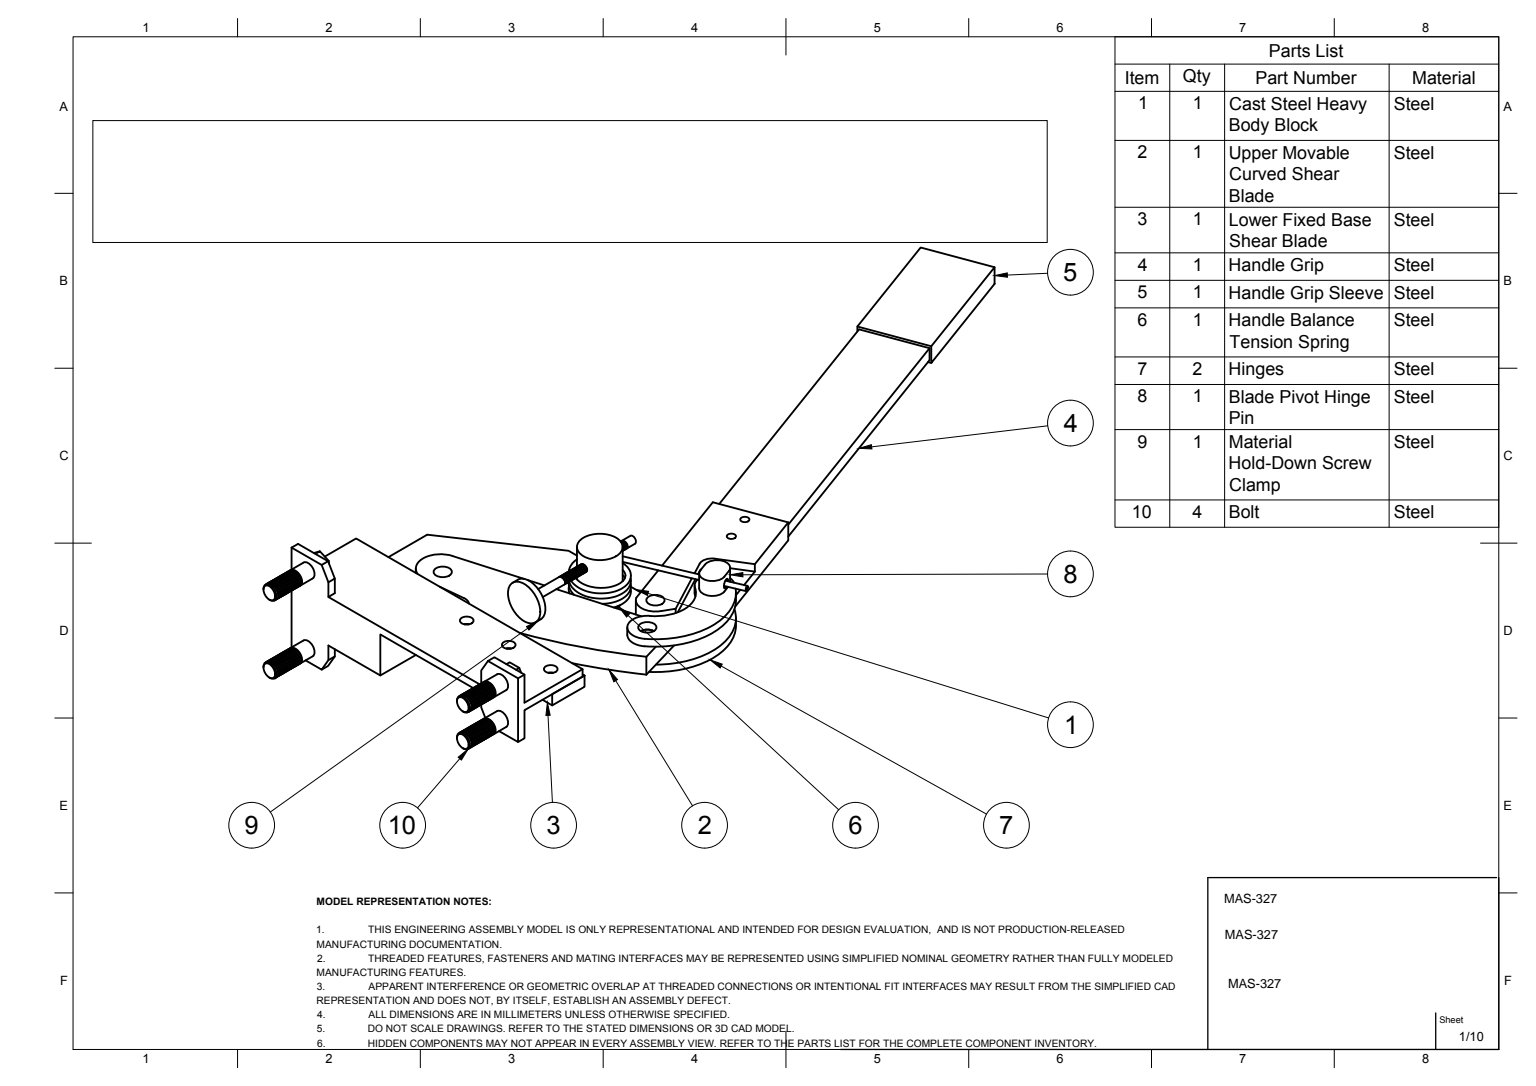
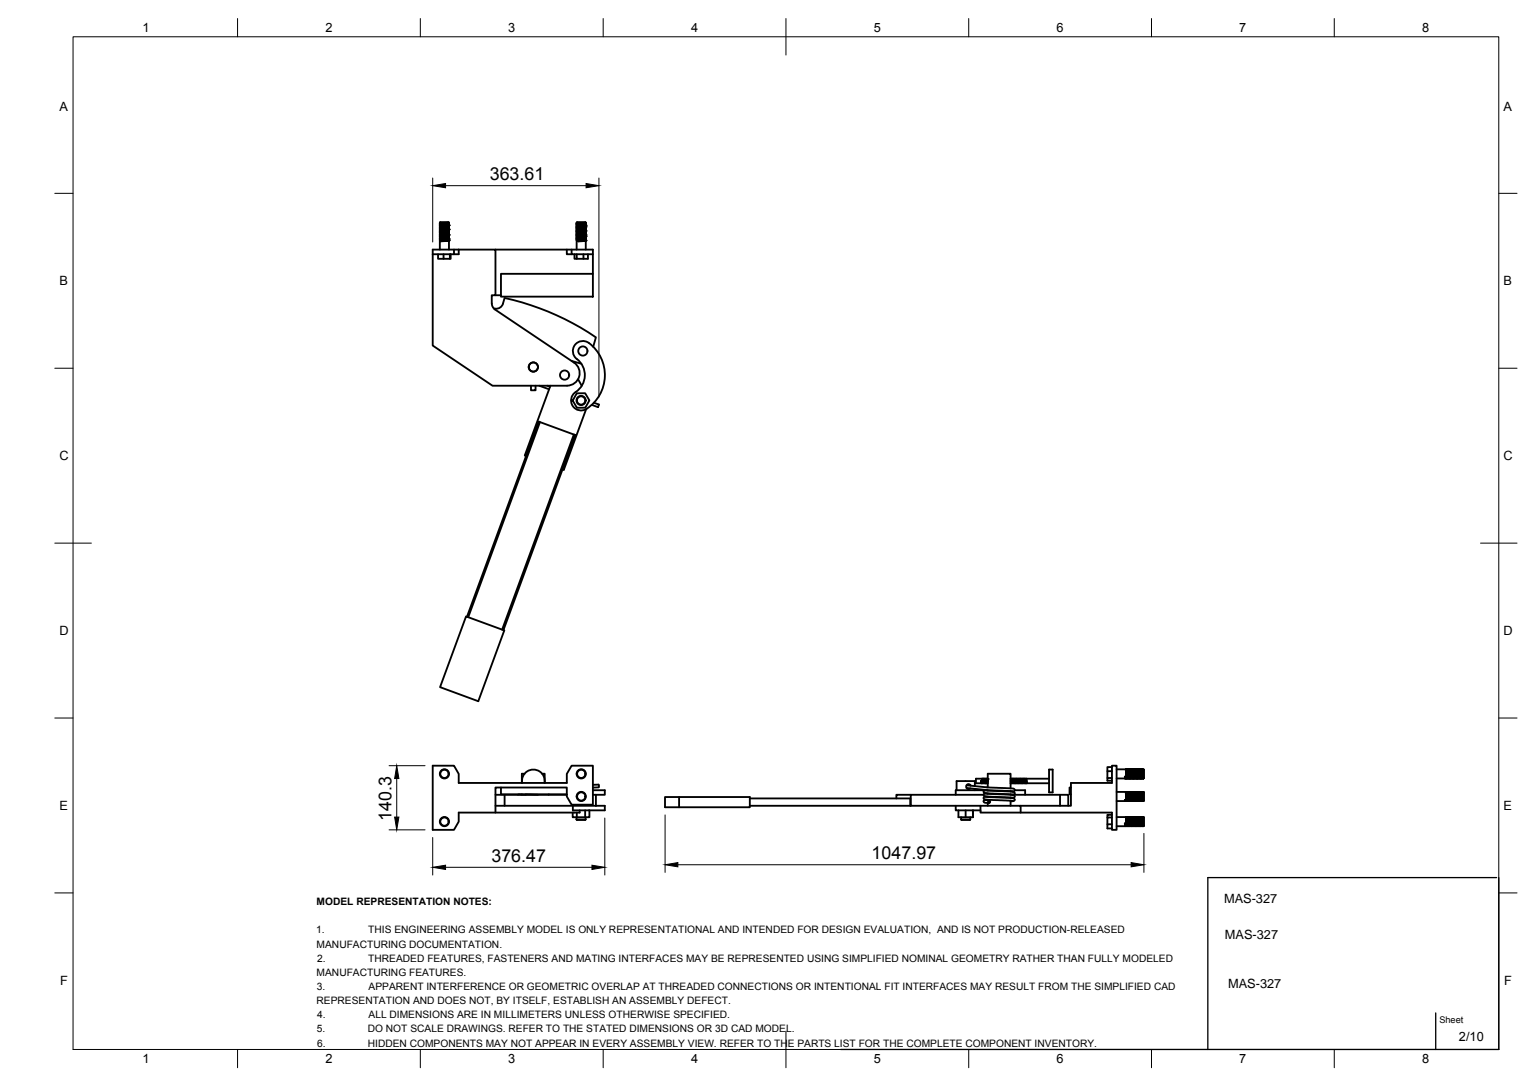
ISO-10303-21;
HEADER;
FILE_DESCRIPTION (('STEP AP214'),
    '1' );
FILE_NAME ('MAS-327',
    '2026-10-06T22:16:42',
    ( '' ),
    ( '' ),
    'SwSTEP 2.0',
    'SolidWorks 2025',
    '' );
FILE_SCHEMA (( 'AUTOMOTIVE_DESIGN' ));
ENDSEC;

DATA;
#1 = CARTESIAN_POINT ( 'NONE',  ( -157.2955611005345986, -176.6084106276440195, 41.63779006702063867 ) ) ;
#2 = ORIENTED_EDGE ( 'NONE', *, *, #5010, .T. ) ;
#3 = CARTESIAN_POINT ( 'NONE',  ( 41.64333658814960870, 63.71518717409399812, 38.42115945441014446 ) ) ;
#4 = CARTESIAN_POINT ( 'NONE',  ( -160.8964159109769696, -164.1584106276440593, 49.65701158161630957 ) ) ;
#5 = CARTESIAN_POINT ( 'NONE',  ( 71.26135857449716582, 118.5824631887579272, 4.723566274445706092 ) ) ;
#6 = FILL_AREA_STYLE_COLOUR ( '', #17600 ) ;
#7 = CARTESIAN_POINT ( 'NONE',  ( 40.27526882409969033, 126.5651871740940209, 37.97664729208901946 ) ) ;
#8 = VERTEX_POINT ( 'NONE', #17420 ) ;
#9 = ORIENTED_EDGE ( 'NONE', *, *, #6823, .T. ) ;
#10 = AXIS2_PLACEMENT_3D ( 'NONE', #19848, #7848, #14551 ) ;
#11 = CARTESIAN_POINT ( 'NONE',  ( -141.4692556286852891, -192.9891397928654726, 49.65701158161630957 ) ) ;
#12 = EDGE_LOOP ( 'NONE', ( #7089, #16124, #17025, #12845, #13237 ) ) ;
#13 = CARTESIAN_POINT ( 'NONE',  ( 41.46631938032478359, 107.1844580088725820, 29.45539723777780239 ) ) ;
#14 = CARTESIAN_POINT ( 'NONE',  ( 38.58424406990786082, 153.3797705074273097, 34.21067981925357060 ) ) ;
#15 = CARTESIAN_POINT ( 'NONE',  ( 44.37947211624943833, 71.47977050742731819, 30.00020018409699318 ) ) ;
#17 = CARTESIAN_POINT ( 'NONE',  ( 22.10153057061799231, 100.9866247252079745, 1.346821830042071566 ) ) ;
#16 = CARTESIAN_POINT ( 'NONE',  ( 39.42975644700377558, 122.8151871740940067, 31.60846029578754468 ) ) ;
#18 = CARTESIAN_POINT ( 'NONE',  ( 39.92123440845004723, 84.26049967264872009, 29.95742577749337343 ) ) ;
#19 = CARTESIAN_POINT ( 'NONE',  ( 8.829984022807513711, 121.7968051057545580, 16.14860047415989541 ) ) ;
#20 = CARTESIAN_POINT ( 'NONE',  ( -136.4581486297550441, -116.9891397928655010, 49.65701158161631668 ) ) ;
#21 = CARTESIAN_POINT ( 'NONE',  ( 157.5268905834513475, 193.0332408774651185, -5.999999999999950262 ) ) ;
#22 = CARTESIAN_POINT ( 'NONE',  ( 44.37947211624943833, 79.01518717409400949, 38.42115945441014446 ) ) ;
#23 = CARTESIAN_POINT ( 'NONE',  ( 39.92123440845005433, 82.16049967264872578, 38.46393386101375711 ) ) ;
#24 = CARTESIAN_POINT ( 'NONE',  ( 41.46631938032478359, 133.3104996726487457, 38.96596240072933170 ) ) ;
#25 = CIRCLE ( 'NONE', #1445, 7.500000000000007105 ) ;
#26 = EDGE_CURVE ( 'NONE', #19406, #2203, #2326, .T. ) ;
#27 = ORIENTED_EDGE ( 'NONE', *, *, #7982, .F. ) ;
#28 = CARTESIAN_POINT ( 'NONE',  ( 44.37947211624943833, 68.47977050742731819, 30.00020018409699318 ) ) ;
#29 = CARTESIAN_POINT ( 'NONE',  ( -154.3824083646099439, -187.5584106276440650, 58.62277379824867296 ) ) ;
#30 = CARTESIAN_POINT ( 'NONE',  ( 39.19820123626366382, 154.0079489008930693, -4.284297094604833767 ) ) ;
#31 = CARTESIAN_POINT ( 'NONE',  ( -154.3824083646099439, -178.5584106276440366, 58.62277379824867296 ) ) ;
#32 = VERTEX_POINT ( 'NONE', #9176 ) ;
#33 = CARTESIAN_POINT ( 'NONE',  ( 38.58424406990786082, 150.1151871740939896, 34.21067981925357060 ) ) ;
#34 = DIRECTION ( 'NONE',  ( 0.4874675571821265319, 0.8731411001063289490, -0.000000000000000000 ) ) ;
#35 = CARTESIAN_POINT ( 'NONE',  ( 43.01140435219951286, 110.6297705074273097, 29.55568802177586107 ) ) ;
#36 = CARTESIAN_POINT ( 'NONE',  ( 47.05648932407426344, 153.9844580088725934, 37.14960608071593384 ) ) ;
#37 = ORIENTED_EDGE ( 'NONE', *, *, #161, .T. ) ;
#38 = PRODUCT_RELATED_PRODUCT_CATEGORY ( 'part', '', ( #19990 ) ) ;
#39 = CARTESIAN_POINT ( 'NONE',  ( 43.64334309031418968, 148.0990856179656419, -3.057864931601543823 ) ) ;
#40 = VERTEX_POINT ( 'NONE', #786 ) ;
#41 = CARTESIAN_POINT ( 'NONE',  ( 45.74753988029933538, 116.3297705074272983, 30.44471234641811819 ) ) ;
#42 = ADVANCED_FACE ( 'NONE', ( #9065 ), #564, .F. ) ;
#43 = CARTESIAN_POINT ( 'NONE',  ( 47.43856463449117200, 157.7651871740939953, 32.77220824515698183 ) ) ;
#44 = CARTESIAN_POINT ( 'NONE',  ( 72.37431012622080573, 137.3510900982057308, 5.986230922049878167 ) ) ;
#45 = CARTESIAN_POINT ( 'NONE',  ( -161.4692556286852607, -176.3391397928654669, 52.90620854394536821 ) ) ;
#46 = ADVANCED_FACE ( 'NONE', ( #7741 ), #6067, .T. ) ;
#47 = CARTESIAN_POINT ( 'NONE',  ( 2.004595370269653287, 635.3380690778678854, -0.8325491102011938205 ) ) ;
#48 = FACE_BOUND ( 'NONE', #8175, .T. ) ;
#49 = CARTESIAN_POINT ( 'NONE',  ( -120.0322075325610598, -126.9891397928655010, -54.65701158161630246 ) ) ;
#50 = ITEM_DEFINED_TRANSFORMATION ( 'NONE', 'NONE', #7761,  #12657 ) ;
#51 = CARTESIAN_POINT ( 'NONE',  ( 43.01140435219954838, 110.9604996726487371, 29.21067981925356705 ) ) ;
#52 = CARTESIAN_POINT ( 'NONE',  ( 38.58424406990786082, 90.37977050742732388, 34.21067981925357060 ) ) ;
#53 = CARTESIAN_POINT ( 'NONE',  ( 58.35211712195835076, 96.24552883246097679, -7.224606741634919338 ) ) ;
#54 = CARTESIAN_POINT ( 'NONE',  ( -142.0420953463936087, -174.3938272943107393, 49.65701158161630957 ) ) ;
#55 = CARTESIAN_POINT ( 'NONE',  ( 38.58424406990786082, 90.11518717409400381, 34.21067981925357060 ) ) ;
#56 = ADVANCED_FACE ( 'NONE', ( #2544 ), #19514, .T. ) ;
#57 = ORIENTED_EDGE ( 'NONE', *, *, #21284, .T. ) ;
#58 = LINE ( 'NONE', #15385, #4469 ) ;
#59 = CARTESIAN_POINT ( 'NONE',  ( 77.24268685965694203, 120.2105100216710696, 12.57728155048203433 ) ) ;
#60 = CARTESIAN_POINT ( 'NONE',  ( 43.01140435219951286, 139.1297705074273097, 38.86567161673127657 ) ) ;
#61 = CARTESIAN_POINT ( 'NONE',  ( 40.36503175183082703, 91.91162403226272204, -5.481956346182379924 ) ) ;
#62 = MANIFOLD_SOLID_BREP ( 'Thread1', #3899 ) ;
#63 = CARTESIAN_POINT ( 'NONE',  ( 43.01140435219951286, 119.0344580088725621, 29.21067981925356705 ) ) ;
#64 =( BOUNDED_CURVE ( )  B_SPLINE_CURVE ( 2, ( #3303, #16737, #14756, #2855, #19725, #1317, #1648, #14970, #11562, #21497, #6273, #9598, #6734 ),
 .UNSPECIFIED., .F., .F. ) 
 B_SPLINE_CURVE_WITH_KNOTS ( ( 3, 2, 2, 2, 2, 2, 3 ),
 ( 0.1249999999999999584, 0.1285714285714285587, 0.1357142857142857040, 0.1428571428571428492, 0.1499999999999999944, 0.1571428571428571397, 0.1607142857142856984 ),
 .UNSPECIFIED. ) 
 CURVE ( )  GEOMETRIC_REPRESENTATION_ITEM ( )  RATIONAL_B_SPLINE_CURVE ( ( 0.9755282581475768211, 0.9755282581475765991, 1.000000000000000000, 0.9510565162951535312, 1.000000000000000000, 0.9510565162951535312, 1.000000000000000000, 0.9510565162951535312, 1.000000000000000000, 0.9510565162951535312, 1.000000000000000000, 0.9755282581475769321, 0.9755282581475768211 ) ) 
 REPRESENTATION_ITEM ( '' )  );
#65 = ORIENTED_EDGE ( 'NONE', *, *, #3046, .T. ) ;
#66 = CARTESIAN_POINT ( 'NONE',  ( 45.74753988029933538, 145.4297705074273210, 37.97664729208901946 ) ) ;
#67 = AXIS2_PLACEMENT_3D ( 'NONE', #12131, #8413, #1572 ) ;
#68 = VECTOR ( 'NONE', #5817, 1000.000000000000000 ) ;
#69 = CARTESIAN_POINT ( 'NONE',  ( 43.01140435219951286, 94.12977050742730967, 38.86567161673127657 ) ) ;
#70 = DIRECTION ( 'NONE',  ( -0.000000000000000000, -0.000000000000000000, 1.000000000000000000 ) ) ;
#71 = CIRCLE ( 'NONE', #14485, 14.42424326798555434 ) ;
#72 = EDGE_CURVE ( 'NONE', #8233, #846, #19303, .T. ) ;
#73 = CARTESIAN_POINT ( 'NONE',  ( 45.22503871336621017, 59.11591952901361680, 30.37667785261832165 ) ) ;
#74 = CARTESIAN_POINT ( 'NONE',  ( -161.4692556286852891, -169.7130981290893317, 46.40781461928724383 ) ) ;
#75 = CARTESIAN_POINT ( 'NONE',  ( -143.3790856849358306, -174.3630981290893089, 55.53486410454105027 ) ) ;
#76 = CARTESIAN_POINT ( 'NONE',  ( 39.92123440845005433, 122.3344580088725593, 29.95742577749336988 ) ) ;
#77 = CARTESIAN_POINT ( 'NONE',  ( -157.6495955161842062, -167.0130981290893146, 41.15050349809590102 ) ) ;
#78 = SHAPE_REPRESENTATION_RELATIONSHIP ( 'NONE' , 'NONE' ,  #6206, #4526 ) ;
#79 = CARTESIAN_POINT ( 'NONE',  ( 46.10157429594899270, 144.8344580088725877, 38.46393386101376421 ) ) ;
#80 = CARTESIAN_POINT ( 'NONE',  ( 39.42975644700377558, 120.6797705074273210, 36.81289934271958941 ) ) ;
#81 = CARTESIAN_POINT ( 'NONE',  ( 15.47577296012077142, 113.4559151263126040, 0.9141320964044082897 ) ) ;
#82 = DIRECTION ( 'NONE',  ( 0.000000000000000000, 0.000000000000000000, -1.000000000000000000 ) ) ;
#83 = CARTESIAN_POINT ( 'NONE',  ( 44.37947211624943833, 121.0151871740940095, 38.42115945441014446 ) ) ;
#84 = VECTOR ( 'NONE', #11009, 1000.000000000000000 ) ;
#86 = DIRECTION ( 'NONE',  ( 0.000000000000000000, 0.000000000000000000, 1.000000000000000000 ) ) ;
#85 = VECTOR ( 'NONE', #7923, 1000.000000000000000 ) ;
#87 = CARTESIAN_POINT ( 'NONE',  ( 16.50170782505827560, 141.4403336307199197, 3.843654360456687513 ) ) ;
#88 = EDGE_CURVE ( 'NONE', #2955, #13896, #17623, .T. ) ;
#89 = CARTESIAN_POINT ( 'NONE',  ( 29.72792815944318789, 144.7825833525567134, 3.370790685444458479 ) ) ;
#90 = LINE ( 'NONE', #6822, #7245 ) ;
#91 = AXIS2_PLACEMENT_3D ( 'NONE', #5623, #16792, #1591 ) ;
#92 = CARTESIAN_POINT ( 'NONE',  ( 41.64333658814960870, 83.77977050742732956, 30.00020018409699318 ) ) ;
#93 = ORIENTED_EDGE ( 'NONE', *, *, #5608, .T. ) ;
#94 = ADVANCED_FACE ( 'NONE', ( #19971 ), #8063, .F. ) ;
#95 = ADVANCED_FACE ( 'NONE', ( #19738 ), #13347, .T. ) ;
#96 = DIRECTION ( 'NONE',  ( -0.000000000000000000, 0.000000000000000000, 1.000000000000000000 ) ) ;
#97 = CARTESIAN_POINT ( 'NONE',  ( 44.55648932407425633, 70.88445800887258486, 29.45539723777780239 ) ) ;
#98 = FACE_OUTER_BOUND ( 'NONE', #3212, .T. ) ;
#99 = CARTESIAN_POINT ( 'NONE',  ( 38.01140435219952707, 132.7104996726487514, 34.21067981925357060 ) ) ;
#101 = CARTESIAN_POINT ( 'NONE',  ( 60.64192606672164487, 149.1585417170215067, -15.56126092485307488 ) ) ;
#100 = CARTESIAN_POINT ( 'NONE',  ( 45.74753988029933538, 89.06518717409399244, 30.44471234641811819 ) ) ;
#102 = CARTESIAN_POINT ( 'NONE',  ( -148.5561028927606344, -162.0584106276440366, 40.69124936498395328 ) ) ;
#103 = CARTESIAN_POINT ( 'NONE',  ( -148.5561028927606344, -192.9938272943107336, 58.62277379824867296 ) ) ;
#104 = DIRECTION ( 'NONE',  ( 0.000000000000000000, 1.000000000000000000, 0.000000000000000000 ) ) ;
#105 = CARTESIAN_POINT ( 'NONE',  ( 43.01140435219951286, 126.5344580088725621, 39.21067981925356349 ) ) ;
#106 = LINE ( 'NONE', #6386, #150 ) ;
#107 = CARTESIAN_POINT ( 'NONE',  ( 46.59305225739526435, 152.1797705074273210, 31.60846029578754468 ) ) ;
#108 = FACE_OUTER_BOUND ( 'NONE', #17831, .T. ) ;
#109 = CARTESIAN_POINT ( 'NONE',  ( 20.88913110926514705, 146.0313881486468119, 3.053432864643822686 ) ) ;
#110 = CARTESIAN_POINT ( 'NONE',  ( 47.43856463449117911, 148.7651871740940237, 32.77220824515697473 ) ) ;
#111 = CARTESIAN_POINT ( 'NONE',  ( -154.3824083646099439, -166.2938272943107165, 58.62277379824867296 ) ) ;
#112 = CARTESIAN_POINT ( 'NONE',  ( -143.8425227516148084, -174.9584106276440707, 55.19815736654470584 ) ) ;
#113 = ORIENTED_EDGE ( 'NONE', *, *, #2599, .F. ) ;
#114 = CARTESIAN_POINT ( 'NONE',  ( -176.9699209214867324, -136.9891397928655010, -72.64809332337415526 ) ) ;
#115 = CARTESIAN_POINT ( 'NONE',  ( -143.8425227516148084, -159.3584106276440480, 44.11586579668791330 ) ) ;
#116 = CARTESIAN_POINT ( 'NONE',  ( 14.84555331229717012, 122.4588817147608637, 1.271029365619425144 ) ) ;
#117 = SURFACE_STYLE_FILL_AREA ( #8505 ) ;
#118 = CARTESIAN_POINT ( 'NONE',  ( 44.37947211624943833, 127.0151871740939953, 38.42115945441014446 ) ) ;
#119 = VERTEX_POINT ( 'NONE', #11350 ) ;
#120 = VERTEX_POINT ( 'NONE', #20084 ) ;
#121 = EDGE_CURVE ( 'NONE', #811, #5132, #2980, .T. ) ;
#122 = CARTESIAN_POINT ( 'NONE',  ( -55.11860757350579831, 784.8075632535900468, -19.99999999999997868 ) ) ;
#123 = ORIENTED_EDGE ( 'NONE', *, *, #17302, .F. ) ;
#124 = CARTESIAN_POINT ( 'NONE',  ( 38.01140435219952707, 98.78445800887259054, 34.21067981925357060 ) ) ;
#125 = CARTESIAN_POINT ( 'NONE',  ( 43.01140435219951286, 154.1297705074273097, 38.86567161673127657 ) ) ;
#126 = CARTESIAN_POINT ( 'NONE',  ( 38.58424406990784661, 63.52977050742730825, 35.64915139335016647 ) ) ;
#128 = CARTESIAN_POINT ( 'NONE',  ( 43.27907770151751521, 148.0257240122537610, -16.07737750751418915 ) ) ;
#127 = CARTESIAN_POINT ( 'NONE',  ( 41.64333658814960870, 114.7151871740940123, 38.42115945441014446 ) ) ;
#129 =( BOUNDED_CURVE ( )  B_SPLINE_CURVE ( 2, ( #10581, #5603, #12328, #19063, #3966, #10688, #17395, #4710, #3061, #19486, #17824, #21366, #12765 ),
 .UNSPECIFIED., .F., .F. ) 
 B_SPLINE_CURVE_WITH_KNOTS ( ( 3, 2, 2, 2, 2, 2, 3 ),
 ( 0.2279411764705882304, 0.2294117647058823428, 0.2323529411764705954, 0.2352941176470588203, 0.2382352941176470451, 0.2411764705882352977, 0.2426470588235294101 ),
 .UNSPECIFIED. ) 
 CURVE ( )  GEOMETRIC_REPRESENTATION_ITEM ( )  RATIONAL_B_SPLINE_CURVE ( ( 0.9755282581475768211, 0.9755282581475768211, 1.000000000000000000, 0.9510565162951535312, 1.000000000000000000, 0.9510565162951535312, 1.000000000000000000, 0.9510565162951535312, 1.000000000000000000, 0.9510565162951535312, 1.000000000000000000, 0.9755282581475768211, 0.9755282581475768211 ) ) 
 REPRESENTATION_ITEM ( '' )  );
#130 = CARTESIAN_POINT ( 'NONE',  ( 38.96631938032478359, 81.41049967264873999, 31.27175355779120025 ) ) ;
#131 = FACE_OUTER_BOUND ( 'NONE', #2097, .T. ) ;
#132 = CARTESIAN_POINT ( 'NONE',  ( -145.2889157411863437, -170.6130981290892805, 41.15050349809589392 ) ) ;
#133 = CARTESIAN_POINT ( 'NONE',  ( 45.51140435220141001, 58.78519719078001060, 29.88055280033245964 ) ) ;
#134 = CARTESIAN_POINT ( 'NONE',  ( 43.01140435219951286, 78.86518717409400381, 38.86567161673127657 ) ) ;
#135 = CARTESIAN_POINT ( 'NONE',  ( 38.96631938032478359, 81.41049967264873999, 31.27175355779120025 ) ) ;
#136 = DIRECTION ( 'NONE',  ( 0.000000000000000000, 0.000000000000000000, 1.000000000000000000 ) ) ;
#137 = VERTEX_POINT ( 'NONE', #11243 ) ;
#138 = CARTESIAN_POINT ( 'NONE',  ( 40.27526882409969033, 65.92977050742732104, 30.44471234641811819 ) ) ;
#139 = CARTESIAN_POINT ( 'NONE',  ( -159.0959885057557983, -190.8584106276440480, 55.19815736654470584 ) ) ;
#140 = CARTESIAN_POINT ( 'NONE',  ( 61.83586340360074018, 91.21788411573329824, -1.307985002297802568 ) ) ;
#141 = CARTESIAN_POINT ( 'NONE',  ( -154.3824083646099439, -173.7584106276440536, 40.69124936498395328 ) ) ;
#142 = ORIENTED_EDGE ( 'NONE', *, *, #6526, .T. ) ;
#143 = CARTESIAN_POINT ( 'NONE',  ( 47.43856463449118621, 154.6151871740940180, 34.21067981925357060 ) ) ;
#144 = CARTESIAN_POINT ( 'NONE',  ( 38.58424406990785371, 158.9651871740939839, 32.77220824515697473 ) ) ;
#145 = CARTESIAN_POINT ( 'NONE',  ( 39.42975644700377558, 117.0797705074273267, 31.60846029578754468 ) ) ;
#146 = CARTESIAN_POINT ( 'NONE',  ( 9.468627745026951814, 113.0646104733145592, 1.862908727141013854 ) ) ;
#147 = EDGE_LOOP ( 'NONE', ( #14360, #18336 ) ) ;
#148 = CARTESIAN_POINT ( 'NONE',  ( 57.39747520560054284, 144.1616143014069280, -9.486357586414486676 ) ) ;
#149 = ORIENTED_EDGE ( 'NONE', *, *, #5345, .F. ) ;
#150 = VECTOR ( 'NONE', #15205, 1000.000000000000000 ) ;
#151 = DIRECTION ( 'NONE',  ( 0.000000000000000000, -1.000000000000000000, 0.000000000000000000 ) ) ;
#152 = CARTESIAN_POINT ( 'NONE',  ( 47.43856463449117200, 86.02977050742731535, 32.77220824515698183 ) ) ;
#153 = CARTESIAN_POINT ( 'NONE',  ( 41.64333658814960870, 152.5151871740940237, 30.00020018409699318 ) ) ;
#154 = CARTESIAN_POINT ( 'NONE',  ( 19.03178791447554374, 95.58698510358173905, 9.200771007679692914 ) ) ;
#155 = FILL_AREA_STYLE_COLOUR ( '', #636 ) ;
#156 = CARTESIAN_POINT ( 'NONE',  ( 131.8222645499857322, 267.5435007770734046, -19.99999999999997868 ) ) ;
#157 = CARTESIAN_POINT ( 'NONE',  ( -141.4692556286852891, -180.9891397928654726, 49.65701158161630957 ) ) ;
#158 = CARTESIAN_POINT ( 'NONE',  ( -154.5594255724347761, -182.1630981290893203, 40.14644641866476604 ) ) ;
#159 = CARTESIAN_POINT ( 'NONE',  ( 138.4260920561042667, 141.9264758756783351, 4.000000000000021316 ) ) ;
#160 = DIRECTION ( 'NONE',  ( -1.000000000000000000, 0.000000000000000000, 0.000000000000000000 ) ) ;
#161 = EDGE_CURVE ( 'NONE', #6406, #8778, #2868, .T. ) ;
#162 = CARTESIAN_POINT ( 'NONE',  ( 38.58424406990784661, 96.52977050742730114, 35.64915139335016647 ) ) ;
#163 = CARTESIAN_POINT ( 'NONE',  ( 16.16443657470430750, 128.5343009702184816, -4.486436360144259616 ) ) ;
#164 = CARTESIAN_POINT ( 'NONE',  ( -143.8425227516148084, -174.0938272943107279, 44.11586579668791330 ) ) ;
#165 = CIRCLE ( 'NONE', #18804, 10.00000000000000888 ) ;
#166 = CARTESIAN_POINT ( 'NONE',  ( 47.43856463449117911, 76.76518717409398107, 32.77220824515697473 ) ) ;
#167 = LINE ( 'NONE', #16491, #14475 ) ;
#168 = DIRECTION ( 'NONE',  ( 0.000000000000000000, 1.000000000000000000, 0.000000000000000000 ) ) ;
#169 = ORIENTED_EDGE ( 'NONE', *, *, #12306, .F. ) ;
#170 = DIRECTION ( 'NONE',  ( 1.000000000000000000, 0.000000000000000000, -0.000000000000000000 ) ) ;
#171 = CARTESIAN_POINT ( 'NONE',  ( 19.13088699441526686, 95.37848931739559077, 15.19637875606281341 ) ) ;
#172 = CARTESIAN_POINT ( 'NONE',  ( 38.58424406990785371, 141.2297705074273040, 32.77220824515697473 ) ) ;
#173 = CARTESIAN_POINT ( 'NONE',  ( 63.17392202723403472, 139.5086487405075673, -1.196242060499778992 ) ) ;
#174 = CARTESIAN_POINT ( 'NONE',  ( 41.64333658814960870, 60.97977050742731109, 38.42115945441014446 ) ) ;
#175 = VERTEX_POINT ( 'NONE', #1443 ) ;
#176 = CARTESIAN_POINT ( 'NONE',  ( 44.37947211624943833, 149.4797705074273324, 30.00020018409699318 ) ) ;
#177 = CARTESIAN_POINT ( 'NONE',  ( 41.64333658814960870, 63.71518717409399812, 38.42115945441014446 ) ) ;
#178 = CARTESIAN_POINT ( 'NONE',  ( -157.6495955161842062, -169.1130981290892805, 58.16351966513671812 ) ) ;
#179 = CARTESIAN_POINT ( 'NONE',  ( -143.8425227516148084, -156.6938272943107222, 55.19815736654470584 ) ) ;
#180 = CARTESIAN_POINT ( 'NONE',  ( 165.8083469658213005, 192.9029763258799335, -44.99999999999997158 ) ) ;
#181 = CARTESIAN_POINT ( 'NONE',  ( -143.3790856849358306, -165.3630981290893089, 55.53486410454105027 ) ) ;
#182 = AXIS2_PLACEMENT_3D ( 'NONE', #12527, #5693, #7365 ) ;
#183 = CARTESIAN_POINT ( 'NONE',  ( 48.01140435219951996, 145.1344580088725991, 35.83527830041810347 ) ) ;
#184 = CARTESIAN_POINT ( 'NONE',  ( 47.43856463449118621, 118.8797705074273239, 34.21067981925357060 ) ) ;
#185 = CARTESIAN_POINT ( 'NONE',  ( 14.84555331229717012, 122.4588817147608637, 1.271029365619425144 ) ) ;
#186 = CARTESIAN_POINT ( 'NONE',  ( 42.21948215057683740, 140.1113394311928744, 29.21067981925357415 ) ) ;
#187 = CARTESIAN_POINT ( 'NONE',  ( 46.59305225739526435, 106.3151871740939924, 36.81289934271958941 ) ) ;
#188 = DIRECTION ( 'NONE',  ( 0.000000000000000000, 1.000000000000000000, 0.000000000000000000 ) ) ;
#189 = CARTESIAN_POINT ( 'NONE',  ( 9.953047844039691228, 128.4882722429139505, 3.367556520687803090 ) ) ;
#190 = CARTESIAN_POINT ( 'NONE',  ( 17.20459894546975832, 108.5405110446994001, 1.704077971530460811 ) ) ;
#191 = CARTESIAN_POINT ( 'NONE',  ( -151.4692556286852607, -155.3130981290892976, 39.65701158161629536 ) ) ;
#192 = EDGE_CURVE ( 'NONE', #1584, #12255, #9504, .T. ) ;
#193 = CARTESIAN_POINT ( 'NONE',  ( 40.27526882409969744, 81.82977050742729830, 37.97664729208901235 ) ) ;
#194 = ADVANCED_FACE ( 'NONE', ( #9612 ), #13126, .F. ) ;
#195 = ORIENTED_EDGE ( 'NONE', *, *, #5906, .T. ) ;
#196 = AXIS2_PLACEMENT_3D ( 'NONE', #10385, #15763, #18755 ) ;
#197 = CARTESIAN_POINT ( 'NONE',  ( -145.2889157411863437, -167.6130981290893089, 41.15050349809589392 ) ) ;
#198 = CARTESIAN_POINT ( 'NONE',  ( 38.96631938032478359, 69.08445800887258770, 37.14960608071593384 ) ) ;
#199 = CARTESIAN_POINT ( 'NONE',  ( 46.10157429594899270, 125.6604996726487542, 29.95742577749337343 ) ) ;
#201 = CARTESIAN_POINT ( 'NONE',  ( 44.01981256007524479, 154.0451711359460774, -9.132611258894215212 ) ) ;
#200 = CARTESIAN_POINT ( 'NONE',  ( 47.43856463449118621, 85.61518717409400381, 34.21067981925357060 ) ) ;
#202 = CARTESIAN_POINT ( 'NONE',  ( -160.8964159109769696, -158.3084106276440650, 46.59394152635518793 ) ) ;
#203 = CARTESIAN_POINT ( 'NONE',  ( -145.6429501568359797, -176.9438272943107506, 41.63779006702063867 ) ) ;
#204 = FACE_OUTER_BOUND ( 'NONE', #7069, .T. ) ;
#205 = CARTESIAN_POINT ( 'NONE',  ( -157.6495955161842062, -194.0130981290893146, 41.15050349809590102 ) ) ;
#206 = AXIS2_PLACEMENT_3D ( 'NONE', #10122, #1740, #19817 ) ;
#207 = CARTESIAN_POINT ( 'NONE',  ( 44.55648932407425633, 68.81049967264874567, 29.45539723777780239 ) ) ;
#208 = CARTESIAN_POINT ( 'NONE',  ( -157.6495955161842062, -173.9391397928654328, 41.15050349809589392 ) ) ;
#209 = CIRCLE ( 'NONE', #14661, 576.1986910693910886 ) ;
#210 = CARTESIAN_POINT ( 'NONE',  ( 38.58424406990786082, 153.3797705074273097, 34.21067981925357060 ) ) ;
#211 = CARTESIAN_POINT ( 'NONE',  ( -151.4692556286852607, -183.8130981290892692, 59.65701158161632378 ) ) ;
#212 = CARTESIAN_POINT ( 'NONE',  ( 23.00888394656308122, 147.7027690514567837, -4.855972970016076751 ) ) ;
#213 = CARTESIAN_POINT ( 'NONE',  ( 44.37947211624943833, 143.2151871740940123, 30.00020018409699318 ) ) ;
#214 = CIRCLE ( 'NONE', #196, 21.47274291077713571 ) ;
#215 = CARTESIAN_POINT ( 'NONE',  ( -151.4692556286852891, -155.6438272943107393, 39.74470866294723947 ) ) ;
#216 = CARTESIAN_POINT ( 'NONE',  ( -148.5561028927606344, -175.2584106276440536, 58.62277379824867296 ) ) ;
#217 = CARTESIAN_POINT ( 'NONE',  ( 38.58424406990785371, 63.26518717409400239, 35.64915139335015937 ) ) ;
#218 = CARTESIAN_POINT ( 'NONE',  ( -154.3824083646099439, -160.5584106276440366, 58.62277379824867296 ) ) ;
#219 = CARTESIAN_POINT ( 'NONE',  ( 26.43292637418678126, 142.8198486544370098, 2.223537717183381002 ) ) ;
#220 = CARTESIAN_POINT ( 'NONE',  ( 83.67254549292280785, -61.68114226949890622, 10.00000000000001599 ) ) ;
#221 = CARTESIAN_POINT ( 'NONE',  ( 47.43856463449117200, 121.4651871740939839, 35.64915139335016647 ) ) ;
#222 = ORIENTED_EDGE ( 'NONE', *, *, #8399, .T. ) ;
#223 = ORIENTED_EDGE ( 'NONE', *, *, #18510, .T. ) ;
#224 = CARTESIAN_POINT ( 'NONE',  ( 42.21948215057684450, 114.4575765865522925, 39.21067981925355639 ) ) ;
#225 = ORIENTED_EDGE ( 'NONE', *, *, #21350, .F. ) ;
#226 = CARTESIAN_POINT ( 'NONE',  ( 39.92123440845004723, 105.2344580088725507, 38.46393386101376421 ) ) ;
#227 = CARTESIAN_POINT ( 'NONE',  ( 46.10157429594899270, 115.7604996726487201, 38.46393386101375711 ) ) ;
#228 = CARTESIAN_POINT ( 'NONE',  ( 41.46631938032478359, 156.1104996726487570, 29.45539723777780239 ) ) ;
#230 = CARTESIAN_POINT ( 'NONE',  ( 33.52710748945926866, 93.34978808121778115, 14.79936193957723312 ) ) ;
#229 = CARTESIAN_POINT ( 'NONE',  ( 40.27526882409969033, 113.6651871740939868, 30.44471234641811819 ) ) ;
#231 = AXIS2_PLACEMENT_3D ( 'NONE', #21325, #21217, #9973 ) ;
#232 = CARTESIAN_POINT ( 'NONE',  ( 41.46631938032478359, 70.31049967264874567, 38.96596240072933170 ) ) ;
#233 = CARTESIAN_POINT ( 'NONE',  ( 38.01140435219952707, 74.78445800887257633, 34.21067981925357060 ) ) ;
#234 = PLANE ( 'NONE',  #15635 ) ;
#235 = CARTESIAN_POINT ( 'NONE',  ( 48.01153233465171866, 95.41220631508043937, 33.88560042642480852 ) ) ;
#236 = CARTESIAN_POINT ( 'NONE',  ( 46.59305225739526435, 76.91518717409400097, 31.60846029578754468 ) ) ;
#237 = DIRECTION ( 'NONE',  ( 0.000000000000000000, 0.000000000000000000, 1.000000000000000000 ) ) ;
#238 = EDGE_CURVE ( 'NONE', #951, #16393, #2471, .T. ) ;
#239 = CARTESIAN_POINT ( 'NONE',  ( -160.8964159109769696, -178.8938272943107393, 49.65701158161630957 ) ) ;
#240 = DIRECTION ( 'NONE',  ( 0.000000000000000000, 0.000000000000000000, 1.000000000000000000 ) ) ;
#241 = ADVANCED_FACE ( 'NONE', ( #14877 ), #10156, .F. ) ;
#242 = ORIENTED_EDGE ( 'NONE', *, *, #18959, .F. ) ;
#243 = CARTESIAN_POINT ( 'NONE',  ( -160.8964159109769696, -185.1584106276440309, 49.65701158161630957 ) ) ;
#244 = AXIS2_PLACEMENT_3D ( 'NONE', #16241, #7884, #6214 ) ;
#245 = CARTESIAN_POINT ( 'NONE',  ( 40.94072057685551869, 85.65469043817564909, -0.5939954219232065347 ) ) ;
#246 = CARTESIAN_POINT ( 'NONE',  ( -159.0959885057557983, -176.4584106276440707, 44.11586579668791330 ) ) ;
#247 = ORIENTED_EDGE ( 'NONE', *, *, #8038, .T. ) ;
#248 = CARTESIAN_POINT ( 'NONE',  ( 45.74753988029933538, 157.1651871740940010, 37.97664729208901946 ) ) ;
#249 = DIRECTION ( 'NONE',  ( 1.000000000000000000, 0.000000000000000000, 4.622506457652817044E-16 ) ) ;
#250 = CARTESIAN_POINT ( 'NONE',  ( 47.43856463449117911, 119.0297705074273296, 32.77220824515697473 ) ) ;
#251 = CARTESIAN_POINT ( 'NONE',  ( 22.46358530849972723, 92.52609567587644790, 8.053519324161520387 ) ) ;
#252 = EDGE_LOOP ( 'NONE', ( #9196, #12169, #13904, #16098 ) ) ;
#253 = CARTESIAN_POINT ( 'NONE',  ( 60.80507725967250821, 98.03074643439879310, -7.343579217248467295 ) ) ;
#254 =( BOUNDED_CURVE ( )  B_SPLINE_CURVE ( 2, ( #11919, #6861, #13567, #11591, #1679, #20305, #3331, #8190, #13469, #21744, #9952, #20201, #18648 ),
 .UNSPECIFIED., .F., .F. ) 
 B_SPLINE_CURVE_WITH_KNOTS ( ( 3, 2, 2, 2, 2, 2, 3 ),
 ( 0.5955882352941176405, 0.5970588235294117530, 0.5999999999999999778, 0.6029411764705882026, 0.6058823529411764275, 0.6088235294117646523, 0.6102941176470587648 ),
 .UNSPECIFIED. ) 
 CURVE ( )  GEOMETRIC_REPRESENTATION_ITEM ( )  RATIONAL_B_SPLINE_CURVE ( ( 0.9755282581475768211, 0.9755282581475768211, 1.000000000000000000, 0.9510565162951535312, 1.000000000000000000, 0.9510565162951535312, 1.000000000000000000, 0.9510565162951535312, 1.000000000000000000, 0.9510565162951535312, 1.000000000000000000, 0.9755282581475777093, 0.9755282581475768211 ) ) 
 REPRESENTATION_ITEM ( '' )  );
#255 = VERTEX_POINT ( 'NONE', #6848 ) ;
#256 = CARTESIAN_POINT ( 'NONE',  ( 45.74753988029933538, 109.4297705074273210, 37.97664729208901946 ) ) ;
#257 = FACE_BOUND ( 'NONE', #16069, .T. ) ;
#258 = CARTESIAN_POINT ( 'NONE',  ( 41.46631938032478359, 128.1844580088725820, 29.45539723777780239 ) ) ;
#259 = CARTESIAN_POINT ( 'NONE',  ( 43.01140435219951286, 82.12977050742730967, 38.86567161673127657 ) ) ;
#260 = CARTESIAN_POINT ( 'NONE',  ( 47.43856463449118621, 145.6151871740939896, 34.21067981925357060 ) ) ;
#261 = VECTOR ( 'NONE', #10869, 1000.000000000000000 ) ;
#262 = CARTESIAN_POINT ( 'NONE',  ( 10.61900875472251649, 108.8314319666055212, -5.279948415675857376 ) ) ;
#263 = CARTESIAN_POINT ( 'NONE',  ( 43.01140435219951286, 83.03445800887257633, 29.21067981925356705 ) ) ;
#264 = CARTESIAN_POINT ( 'NONE',  ( 109.8528842077358405, 344.7014318495014322, 4.000000000000003553 ) ) ;
#265 = CARTESIAN_POINT ( 'NONE',  ( -143.3790856849358306, -171.6891397928654897, 43.77915905869157598 ) ) ;
#266 = CARTESIAN_POINT ( 'NONE',  ( 48.01140435219951996, 101.2104996726487514, 34.21067981925357060 ) ) ;
#267 = CARTESIAN_POINT ( 'NONE',  ( 109.8528842077358405, 344.7014318495014322, 272.0939500981630204 ) ) ;
#268 = EDGE_CURVE ( 'NONE', #2815, #21594, #20508, .T. ) ;
#269 = DIRECTION ( 'NONE',  ( 0.000000000000000000, 0.000000000000000000, 1.000000000000000000 ) ) ;
#270 = DIRECTION ( 'NONE',  ( -0.000000000000000000, -0.000000000000000000, -1.000000000000000000 ) ) ;
#271 = CARTESIAN_POINT ( 'NONE',  ( 44.37947211624943833, 94.27977050742731535, 38.42115945441014446 ) ) ;
#272 = CARTESIAN_POINT ( 'NONE',  ( 46.66836841558743032, 147.8683539324387368, -2.938892455568735240 ) ) ;
#273 = CARTESIAN_POINT ( 'NONE',  ( -157.2955611005346270, -173.3438272943107279, 41.63779006702063867 ) ) ;
#274 = CARTESIAN_POINT ( 'NONE',  ( 44.37947211624943833, 82.01518717409400949, 38.42115945441014446 ) ) ;
#276 = VECTOR ( 'NONE', #19328, 1000.000000000000000 ) ;
#275 = CARTESIAN_POINT ( 'NONE',  ( 173.3794444120442506, -34.13255853780189142, 5.000000000000018652 ) ) ;
#277 = CARTESIAN_POINT ( 'NONE',  ( -161.4692556286852891, -158.6391397928655067, 46.40781461928724383 ) ) ;
#278 = ORIENTED_EDGE ( 'NONE', *, *, #11475, .T. ) ;
#279 = CARTESIAN_POINT ( 'NONE',  ( 41.46631938032478359, 137.1844580088725820, 29.45539723777780239 ) ) ;
#280 = DIRECTION ( 'NONE',  ( -0.000000000000000000, -0.000000000000000000, -1.000000000000000000 ) ) ;
#281 = CARTESIAN_POINT ( 'NONE',  ( 47.43856463449118621, 142.8797705074273381, 34.21067981925357060 ) ) ;
#282 = CARTESIAN_POINT ( 'NONE',  ( 68.61421220432494295, 108.2796574941523886, 7.137043325852385323 ) ) ;
#283 = MANIFOLD_SOLID_BREP ( 'Cut-Extrude11', #13403 ) ;
#284 = ORIENTED_EDGE ( 'NONE', *, *, #3313, .F. ) ;
#285 = VECTOR ( 'NONE', #20979, 1000.000000000000000 ) ;
#286 = CARTESIAN_POINT ( 'NONE',  ( 38.01140435219952707, 119.9344580088725820, 35.83527830041809636 ) ) ;
#287 = ORIENTED_EDGE ( 'NONE', *, *, #12395, .T. ) ;
#288 = CARTESIAN_POINT ( 'NONE',  ( 39.42975644700377558, 135.6797705074273210, 36.81289934271958941 ) ) ;
#289 = APPLICATION_CONTEXT ( 'automotive_design' ) ;
#290 = CARTESIAN_POINT ( 'NONE',  ( 39.92123440845005433, 141.2604996726487627, 29.95742577749336988 ) ) ;
#291 = CARTESIAN_POINT ( 'NONE',  ( 163.1026836591718734, 192.4288937294299160, 34.00000000000001421 ) ) ;
#292 = CARTESIAN_POINT ( 'NONE',  ( 163.3401611601854029, 191.7221236944928364, 21.73429951086134082 ) ) ;
#293 = DIRECTION ( 'NONE',  ( -0.9609212714474144601, -0.2768218020313507610, 0.000000000000000000 ) ) ;
#294 = CARTESIAN_POINT ( 'NONE',  ( -149.8854112254399809, -173.3899795514095388, 39.65701158161628825 ) ) ;
#295 = CARTESIAN_POINT ( 'NONE',  ( 42.21948215057684450, 108.0373810949689926, 29.21067981925356705 ) ) ;
#296 = CARTESIAN_POINT ( 'NONE',  ( -148.3790856849358306, -173.4630981290893033, 40.14644641866477315 ) ) ;
#297 = CARTESIAN_POINT ( 'NONE',  ( -60.08805807470707094, 2.775557561562891351E-14, -185.2641742241206657 ) ) ;
#298 = CARTESIAN_POINT ( 'NONE',  ( 43.01140435219954838, 110.0344580088725763, 29.21067981925356705 ) ) ;
#299 = CARTESIAN_POINT ( 'NONE',  ( 38.01140435219951996, 143.9344580088725536, 35.83527830041810347 ) ) ;
#300 = CARTESIAN_POINT ( 'NONE',  ( 47.43856463449117200, 127.7297705074272898, 35.64915139335016647 ) ) ;
#301 = CARTESIAN_POINT ( 'NONE',  ( 58.57740969237692497, 96.29577388269515836, -1.228997851713355072 ) ) ;
#302 = CARTESIAN_POINT ( 'NONE',  ( 43.01140435219951286, 99.53445800887257633, 39.21067981925356349 ) ) ;
#303 = CARTESIAN_POINT ( 'NONE',  ( 40.27526882409969744, 105.5651871740939782, 37.97664729208901235 ) ) ;
#304 = CARTESIAN_POINT ( 'NONE',  ( 27.25521010731993243, 314.3399865783788414, -19.99999999999996092 ) ) ;
#305 = EDGE_CURVE ( 'NONE', #10554, #5083, #3643, .T. ) ;
#306 = CARTESIAN_POINT ( 'NONE',  ( 15.75986397150585816, 99.18880659646561071, -5.637120474378671808 ) ) ;
#307 = CARTESIAN_POINT ( 'NONE',  ( 40.57367117788501787, 91.81261228707245436, 0.5136478283763052932 ) ) ;
#308 = CARTESIAN_POINT ( 'NONE',  ( -145.2889157411863437, -156.5130981290893146, 58.16351966513671812 ) ) ;
#309 = CARTESIAN_POINT ( 'NONE',  ( 38.58424406990785371, 90.22977050742731819, 32.77220824515697473 ) ) ;
#310 = VERTEX_POINT ( 'NONE', #11904 ) ;
#311 = CARTESIAN_POINT ( 'NONE',  ( 43.01140435219954838, 109.4604996726487371, 39.21067981925356349 ) ) ;
#312 = CARTESIAN_POINT ( 'NONE',  ( 48.01140435219951996, 76.13445800887258486, 35.83527830041810347 ) ) ;
#313 = CARTESIAN_POINT ( 'NONE',  ( 38.01140435219952707, 59.63445800887256354, 32.58608133808903773 ) ) ;
#315 = EDGE_CURVE ( 'NONE', #5215, #4975, #25, .T. ) ;
#314 = CARTESIAN_POINT ( 'NONE',  ( 44.55648932407425633, 128.8104996726487457, 29.45539723777780239 ) ) ;
#316 = CARTESIAN_POINT ( 'NONE',  ( 38.58424406990784661, 87.26518717409399528, 35.64915139335016647 ) ) ;
#317 = CARTESIAN_POINT ( 'NONE',  ( -151.4692556286852891, -155.9084106276440593, 39.74470866294723947 ) ) ;
#318 = CARTESIAN_POINT ( 'NONE',  ( -142.0420953463936087, -177.3938272943107393, 49.65701158161630957 ) ) ;
#319 = CARTESIAN_POINT ( 'NONE',  ( -143.3790856849358306, -177.6891397928654612, 43.77915905869157598 ) ) ;
#320 = CARTESIAN_POINT ( 'NONE',  ( -143.3790856849358306, -194.7630981290893146, 43.77915905869157598 ) ) ;
#321 = CARTESIAN_POINT ( 'NONE',  ( 38.01140435219952707, 92.78445800887257633, 34.21067981925357060 ) ) ;
#322 = CARTESIAN_POINT ( 'NONE',  ( 48.01140435219951996, 143.0604996726487457, 35.83527830041809636 ) ) ;
#323 = CARTESIAN_POINT ( 'NONE',  ( 41.64333658814960870, 149.7797705074273154, 30.00020018409699318 ) ) ;
#324 = CARTESIAN_POINT ( 'NONE',  ( 38.58424406990786082, 108.3797705074273239, 34.21067981925357060 ) ) ;
#325 = EDGE_CURVE ( 'NONE', #14663, #14927, #19896, .T. ) ;
#326 = CARTESIAN_POINT ( 'NONE',  ( 77.24268685965694203, 120.2105100216710696, 12.57728155048203433 ) ) ;
#327 = CARTESIAN_POINT ( 'NONE',  ( 39.42975644700377558, 138.4151871740940010, 36.81289934271958941 ) ) ;
#328 = FACE_OUTER_BOUND ( 'NONE', #18449, .T. ) ;
#329 = CARTESIAN_POINT ( 'NONE',  ( -151.4692556286852891, -176.9084106276440309, 39.74470866294723947 ) ) ;
#330 = VECTOR ( 'NONE', #1964, 1000.000000000000000 ) ;
#331 = CARTESIAN_POINT ( 'NONE',  ( 46.10157429594899270, 90.83445800887255928, 38.46393386101375711 ) ) ;
#332 = CARTESIAN_POINT ( 'NONE',  ( 31.11878897118147336, 145.5659923423516773, -4.562434011626001151 ) ) ;
#333 = EDGE_CURVE ( 'NONE', #19172, #12901, #10944, .T. ) ;
#334 = PRESENTATION_STYLE_ASSIGNMENT (( #15435 ) ) ;
#335 = CARTESIAN_POINT ( 'NONE',  ( 47.43856463449117200, 115.4651871740940123, 35.64915139335016647 ) ) ;
#336 = EDGE_LOOP ( 'NONE', ( #11033, #17342, #3726, #11219 ) ) ;
#337 = ORIENTED_EDGE ( 'NONE', *, *, #13071, .F. ) ;
#338 = DIRECTION ( 'NONE',  ( 0.000000000000000000, 0.000000000000000000, 1.000000000000000000 ) ) ;
#339 = ORIENTED_EDGE ( 'NONE', *, *, #6596, .T. ) ;
#340 = CARTESIAN_POINT ( 'NONE',  ( 48.01140435219951996, 97.43445800887256780, 32.58608133808903773 ) ) ;
#341 = CARTESIAN_POINT ( 'NONE',  ( 47.43856463449117911, 158.0297705074273438, 32.77220824515697473 ) ) ;
#342 = EDGE_CURVE ( 'NONE', #19257, #8316, #5649, .T. ) ;
#343 =( GEOMETRIC_REPRESENTATION_CONTEXT ( 3 ) GLOBAL_UNCERTAINTY_ASSIGNED_CONTEXT ( ( #15680 ) ) GLOBAL_UNIT_ASSIGNED_CONTEXT ( ( #12211, #2186, #7269 ) ) REPRESENTATION_CONTEXT ( 'NONE', 'WORKASPACE' ) );
#344 = CARTESIAN_POINT ( 'NONE',  ( 46.59305225739526435, 62.17977050742732104, 31.60846029578754468 ) ) ;
#346 = CARTESIAN_POINT ( 'NONE',  ( 42.37836782381873491, 91.71465960395167372, 14.44224817795539373 ) ) ;
#345 = CARTESIAN_POINT ( 'NONE',  ( 45.74753988029933538, 118.1651871740939725, 37.97664729208901946 ) ) ;
#347 = CARTESIAN_POINT ( 'NONE',  ( 48.01140435219951996, 71.21049967264873715, 34.21067981925357060 ) ) ;
#348 = LINE ( 'NONE', #7078, #20330 ) ;
#349 = EDGE_CURVE ( 'NONE', #7574, #19197, #1660, .T. ) ;
#350 = CARTESIAN_POINT ( 'NONE',  ( 42.21948215057684450, 123.0373810949690210, 29.21067981925356705 ) ) ;
#351 = CARTESIAN_POINT ( 'NONE',  ( 48.01127559942236900, 95.41215390922535278, 34.53968432338328398 ) ) ;
#352 = CARTESIAN_POINT ( 'NONE',  ( 46.59305225739526435, 73.91518717409400097, 31.60846029578754468 ) ) ;
#353 = MANIFOLD_SOLID_BREP ( 'Cut-Extrude12', #11261 ) ;
#354 = DIRECTION ( 'NONE',  ( 0.000000000000000000, 0.000000000000000000, 1.000000000000000000 ) ) ;
#355 = CARTESIAN_POINT ( 'NONE',  ( -145.6429501568359797, -179.9438272943107506, 41.63779006702063867 ) ) ;
#356 = CARTESIAN_POINT ( 'NONE',  ( 42.21948215057684450, 132.0373810949690210, 29.21067981925355994 ) ) ;
#357 = ORIENTED_EDGE ( 'NONE', *, *, #9562, .T. ) ;
#358 = CARTESIAN_POINT ( 'NONE',  ( -157.2955611005346270, -184.7084106276440423, 57.67623309621198047 ) ) ;
#359 = CARTESIAN_POINT ( 'NONE',  ( 62.34613790317991544, 148.1570561279473850, 11.50573666851796339 ) ) ;
#360 = CARTESIAN_POINT ( 'NONE',  ( -160.8964159109769696, -176.1584106276440309, 49.65701158161630957 ) ) ;
#361 = ORIENTED_EDGE ( 'NONE', *, *, #11790, .F. ) ;
#362 = CARTESIAN_POINT ( 'NONE',  ( 38.58424406990786082, 141.1151871740939896, 34.21067981925357060 ) ) ;
#363 = CARTESIAN_POINT ( 'NONE',  ( 18.67254549292281496, -61.68114226949890622, 10.00000000000001599 ) ) ;
#364 = EDGE_CURVE ( 'NONE', #13608, #15461, #11277, .T. ) ;
#365 = CARTESIAN_POINT ( 'NONE',  ( 46.59305225739526435, 106.5797705074273125, 36.81289934271958941 ) ) ;
#366 = CARTESIAN_POINT ( 'NONE',  ( 8.869018199820361659, 117.4101421016551967, 9.005765870029716069 ) ) ;
#367 = ORIENTED_EDGE ( 'NONE', *, *, #11936, .F. ) ;
#368 = CARTESIAN_POINT ( 'NONE',  ( 50.21395344324809429, 147.1711500555979626, 4.203964687196366512 ) ) ;
#369 = EDGE_LOOP ( 'NONE', ( #21532, #16154, #367, #8720 ) ) ;
#370 = CARTESIAN_POINT ( 'NONE',  ( 43.01140435219951996, 10.71049967264875491, 34.21067981925357060 ) ) ;
#371 = CARTESIAN_POINT ( 'NONE',  ( 0.08333186253070556937, 634.6318465664363657, -3.999999999999996447 ) ) ;
#372 = CARTESIAN_POINT ( 'NONE',  ( 47.43856463449117200, 148.4651871740940123, 35.64915139335016647 ) ) ;
#373 = CARTESIAN_POINT ( 'NONE',  ( 43.01140435219951286, 98.96049967264872294, 28.95336869806222779 ) ) ;
#374 = CARTESIAN_POINT ( 'NONE',  ( 29.43094928344231320, 88.48265962617873015, 0.7917390523231137012 ) ) ;
#375 = CLOSED_SHELL ( 'NONE', ( #8062, #8739, #16372, #2106, #6229, #2878, #10037, #18884, #18118, #3960, #13156, #6514, #20224, #19647 ) ) ;
#376 = CARTESIAN_POINT ( 'NONE',  ( -141.4692556286852891, -179.9130981290893203, 46.40781461928724383 ) ) ;
#377 = CARTESIAN_POINT ( 'NONE',  ( -161.4692556286853176, -167.4891397928654726, 49.65701158161630957 ) ) ;
#378 = LINE ( 'NONE', #18569, #11533 ) ;
#379 = CARTESIAN_POINT ( 'NONE',  ( -153.0531000319306827, -193.8160212151857706, 59.65701158161632378 ) ) ;
#380 = FACE_OUTER_BOUND ( 'NONE', #4715, .T. ) ;
#381 = CARTESIAN_POINT ( 'NONE',  ( 44.37947211624943833, 89.47977050742731819, 30.00020018409699318 ) ) ;
#382 = CARTESIAN_POINT ( 'NONE',  ( 71.13433436327568415, 121.9840874124550965, -8.414894741535439593 ) ) ;
#383 = CARTESIAN_POINT ( 'NONE',  ( -145.6429501568359797, -176.9438272943107506, 41.63779006702063867 ) ) ;
#384 = CARTESIAN_POINT ( 'NONE',  ( 40.27526882409969744, 74.66518717409398675, 30.44471234641812174 ) ) ;
#385 = CARTESIAN_POINT ( 'NONE',  ( 147.5268905834513475, 193.0332408774651185, -50.99999999999998579 ) ) ;
#386 = DIRECTION ( 'NONE',  ( -1.000000000000000000, 0.000000000000000000, 0.000000000000000000 ) ) ;
#387 = ORIENTED_EDGE ( 'NONE', *, *, #9191, .T. ) ;
#388 = CARTESIAN_POINT ( 'NONE',  ( 43.01140435219951286, 118.4604996726487371, 39.21067981925356349 ) ) ;
#389 = CARTESIAN_POINT ( 'NONE',  ( 48.01140435219951996, 122.3604996726487428, 32.58608133808903773 ) ) ;
#390 =( BOUNDED_CURVE ( )  B_SPLINE_CURVE ( 2, ( #14473, #19664, #17996, #21660, #9644, #6210, #4442, #6436, #18109, #9860, #13273, #13160, #19889 ),
 .UNSPECIFIED., .F., .F. ) 
 B_SPLINE_CURVE_WITH_KNOTS ( ( 3, 2, 2, 2, 2, 2, 3 ),
 ( 0.8455882352941176405, 0.8470588235294117530, 0.8499999999999999778, 0.8529411764705882026, 0.8558823529411764275, 0.8588235294117646523, 0.8602941176470588758 ),
 .UNSPECIFIED. ) 
 CURVE ( )  GEOMETRIC_REPRESENTATION_ITEM ( )  RATIONAL_B_SPLINE_CURVE ( ( 0.9755282581475768211, 0.9755282581475768211, 1.000000000000000000, 0.9510565162951535312, 1.000000000000000000, 0.9510565162951535312, 1.000000000000000000, 0.9510565162951535312, 1.000000000000000000, 0.9510565162951535312, 1.000000000000000000, 0.9755282581475758219, 0.9755282581475768211 ) ) 
 REPRESENTATION_ITEM ( '' )  );
#391 = CARTESIAN_POINT ( 'NONE',  ( 47.43856463449118621, 133.8797705074273381, 34.21067981925357060 ) ) ;
#392 = CARTESIAN_POINT ( 'NONE',  ( 53.81137604271221164, 145.8702381773545653, 5.351212940250758443 ) ) ;
#393 = VERTEX_POINT ( 'NONE', #13983 ) ;
#394 = LINE ( 'NONE', #7017, #18876 ) ;
#395 = EDGE_LOOP ( 'NONE', ( #15244, #20080, #9642, #2712 ) ) ;
#396 = CARTESIAN_POINT ( 'NONE',  ( 41.64333658814960870, 132.9797705074273324, 38.42115945441014446 ) ) ;
#397 = ADVANCED_FACE ( 'NONE', ( #5931 ), #9362, .T. ) ;
#398 = CARTESIAN_POINT ( 'NONE',  ( 44.37947211624943833, 92.47977050742731819, 30.00020018409699318 ) ) ;
#399 = CARTESIAN_POINT ( 'NONE',  ( 40.27526882409969033, 59.66518717409400097, 30.44471234641811819 ) ) ;
#400 = DIRECTION ( 'NONE',  ( 1.000000000000000000, 0.000000000000000000, 0.000000000000000000 ) ) ;
#401 = CARTESIAN_POINT ( 'NONE',  ( -148.3790856849358306, -192.6630981290892919, 59.16757674456786020 ) ) ;
#402 = CARTESIAN_POINT ( 'NONE',  ( 40.27526882409969033, 93.56518717409397823, 37.97664729208901946 ) ) ;
#403 = CARTESIAN_POINT ( 'NONE',  ( 42.21948215057683740, 154.3836182503284817, 39.21067981925355639 ) ) ;
#404 = CARTESIAN_POINT ( 'NONE',  ( 42.21948215057684450, 122.1113394311928460, 29.21067981925356705 ) ) ;
#405 = CARTESIAN_POINT ( 'NONE',  ( -154.5594255724347761, -173.1630981290893203, 40.14644641866476604 ) ) ;
#406 = DIRECTION ( 'NONE',  ( 1.000000000000000000, 0.000000000000000000, 0.000000000000000000 ) ) ;
#407 = CARTESIAN_POINT ( 'NONE',  ( 44.55648932407425633, 145.8844580088725991, 29.45539723777780239 ) ) ;
#408 = CARTESIAN_POINT ( 'NONE',  ( 45.74753988029933538, 110.3297705074273125, 30.44471234641811819 ) ) ;
#409 = CARTESIAN_POINT ( 'NONE',  ( 31.65106594408818097, 87.52743543124788062, 20.71565594656193454 ) ) ;
#410 = CARTESIAN_POINT ( 'NONE',  ( 145.5008360144876747, 198.5836349573982886, 14.00000000000001776 ) ) ;
#411 = CARTESIAN_POINT ( 'NONE',  ( 39.42975644700377558, 111.4151871740940010, 36.81289934271958941 ) ) ;
#412 = LINE ( 'NONE', #12191, #11898 ) ;
#413 = CARTESIAN_POINT ( 'NONE',  ( 21.78317867943344766, 93.15162560046918827, 9.081842247139665147 ) ) ;
#414 = CARTESIAN_POINT ( 'NONE',  ( 67.15412698936957270, 134.4792784496449087, 12.06138812558265805 ) ) ;
#415 = DIRECTION ( 'NONE',  ( -0.000000000000000000, 1.000000000000000000, -0.000000000000000000 ) ) ;
#416 = CARTESIAN_POINT ( 'NONE',  ( 44.37947211624943833, 88.27977050742731535, 38.42115945441014446 ) ) ;
#417 = VERTEX_POINT ( 'NONE', #9257 ) ;
#418 = CIRCLE ( 'NONE', #12730, 27.58651506682278765 ) ;
#419 = CARTESIAN_POINT ( 'NONE',  ( 47.05648932407426344, 75.98445800887257917, 37.14960608071593384 ) ) ;
#420 = CARTESIAN_POINT ( 'NONE',  ( -145.2889157411863437, -172.4391397928654612, 58.16351966513671812 ) ) ;
#421 = CARTESIAN_POINT ( 'NONE',  ( 44.55648932407425633, 131.8104996726487457, 29.45539723777780239 ) ) ;
#423 = CARTESIAN_POINT ( 'NONE',  ( 10.57123148683770175, 130.5870355106474108, -10.56118268746274325 ) ) ;
#422 = CARTESIAN_POINT ( 'NONE',  ( 47.43856463449117200, 88.76518717409399528, 32.77220824515698183 ) ) ;
#424 = CARTESIAN_POINT ( 'NONE',  ( -159.0959885057557983, -158.4584106276440423, 44.11586579668791330 ) ) ;
#425 = CARTESIAN_POINT ( 'NONE',  ( -160.8964159109769696, -184.8938272943107393, 49.65701158161630957 ) ) ;
#426 = FACE_OUTER_BOUND ( 'NONE', #6664, .T. ) ;
#427 = CARTESIAN_POINT ( 'NONE',  ( 43.01140435219951996, 10.71049967264875491, 39.21067981925356349 ) ) ;
#428 = AXIS2_PLACEMENT_3D ( 'NONE', #10499, #19300, #5628 ) ;
#429 = VECTOR ( 'NONE', #16565, 1000.000000000000000 ) ;
#430 = CYLINDRICAL_SURFACE ( 'NONE', #1907, 10.00000000000000888 ) ;
#431 = DIRECTION ( 'NONE',  ( 0.000000000000000000, 0.000000000000000000, 1.000000000000000000 ) ) ;
#432 = CARTESIAN_POINT ( 'NONE',  ( 46.59305225739526435, 154.5797705074273267, 36.81289934271958941 ) ) ;
#433 = CARTESIAN_POINT ( 'NONE',  ( 38.58424406990786082, 105.3797705074273239, 34.21067981925357060 ) ) ;
#434 = CARTESIAN_POINT ( 'NONE',  ( 68.80033453084351436, 142.5431462587704061, -3.212652714419679700 ) ) ;
#435 = CARTESIAN_POINT ( 'NONE',  ( 38.58424406990786082, 135.1151871740940180, 34.21067981925357060 ) ) ;
#436 = CIRCLE ( 'NONE', #15899, 10.00000000000000888 ) ;
#437 = PLANE ( 'NONE',  #12824 ) ;
#438 = CARTESIAN_POINT ( 'NONE',  ( -160.8964159109769696, -170.0084106276440252, 52.72008163687743121 ) ) ;
#439 = LINE ( 'NONE', #539, #1132 ) ;
#440 = CARTESIAN_POINT ( 'NONE',  ( 58.08784223975295902, 95.98046199469133910, 5.794885020722011504 ) ) ;
#441 = DIRECTION ( 'NONE',  ( 0.000000000000000000, 0.000000000000000000, -1.000000000000000000 ) ) ;
#442 = CARTESIAN_POINT ( 'NONE',  ( 38.58424406990786082, 117.1151871740940038, 34.21067981925357060 ) ) ;
#443 = ORIENTED_EDGE ( 'NONE', *, *, #13738, .F. ) ;
#444 = DIRECTION ( 'NONE',  ( -0.000000000000000000, -0.000000000000000000, 1.000000000000000000 ) ) ;
#445 = ORIENTED_EDGE ( 'NONE', *, *, #15692, .F. ) ;
#446 = ADVANCED_FACE ( 'NONE', ( #16065 ), #9041, .T. ) ;
#447 = CARTESIAN_POINT ( 'NONE',  ( 38.96631938032478359, 102.0844580088725877, 37.14960608071593384 ) ) ;
#448 = CARTESIAN_POINT ( 'NONE',  ( 39.92123440845004723, 154.1604996726487400, 38.46393386101376421 ) ) ;
#450 = CARTESIAN_POINT ( 'NONE',  ( 32.23767430054685690, 145.5917660130465379, 17.43780275515692679 ) ) ;
#449 = CARTESIAN_POINT ( 'NONE',  ( 47.43856463449117200, 115.7651871740939811, 32.77220824515698183 ) ) ;
#451 = CARTESIAN_POINT ( 'NONE',  ( 43.01140435219951286, 68.96049967264870872, 28.95336869806222779 ) ) ;
#453 = CARTESIAN_POINT ( 'NONE',  ( 47.05648932407426344, 148.5844580088725877, 31.27175355779120025 ) ) ;
#452 = DIRECTION ( 'NONE',  ( 0.000000000000000000, 0.000000000000000000, 1.000000000000000000 ) ) ;
#454 = DIRECTION ( 'NONE',  ( 0.3450121214752279175, -0.9385982292947087080, 0.000000000000000000 ) ) ;
#455 = DIRECTION ( 'NONE',  ( 0.000000000000000000, 0.000000000000000000, 1.000000000000000000 ) ) ;
#456 = CARTESIAN_POINT ( 'NONE',  ( 45.74753988029933538, 80.06518717409397823, 30.44471234641811819 ) ) ;
#457 = LINE ( 'NONE', #7188, #7476 ) ;
#458 = CARTESIAN_POINT ( 'NONE',  ( -159.0959885057557983, -185.1938272943107222, 44.11586579668791330 ) ) ;
#459 = DIRECTION ( 'NONE',  ( 0.000000000000000000, 0.000000000000000000, 1.000000000000000000 ) ) ;
#460 = VERTEX_POINT ( 'NONE', #20827 ) ;
#461 = CARTESIAN_POINT ( 'NONE',  ( -143.8425227516148084, -177.9584106276440707, 55.19815736654470584 ) ) ;
#462 = CARTESIAN_POINT ( 'NONE',  ( 52.46025766099742071, 152.8098426157893925, 11.14871012209260748 ) ) ;
#463 = ORIENTED_EDGE ( 'NONE', *, *, #5564, .F. ) ;
#464 = CARTESIAN_POINT ( 'NONE',  ( 43.01140435219951286, 143.3651871740939896, 29.55568802177586463 ) ) ;
#465 = PLANE ( 'NONE',  #7815 ) ;
#466 = CARTESIAN_POINT ( 'NONE',  ( 41.64333658814960870, 102.9797705074273182, 38.42115945441014446 ) ) ;
#467 = CARTESIAN_POINT ( 'NONE',  ( 40.02721236285810136, 85.80382532021769748, 0.4343372985580923329 ) ) ;
#468 = ORIENTED_EDGE ( 'NONE', *, *, #12037, .F. ) ;
#469 = CARTESIAN_POINT ( 'NONE',  ( 41.25620118372704326, 148.0523446076144580, 3.846850258842608117 ) ) ;
#470 = VERTEX_POINT ( 'NONE', #5719 ) ;
#471 = ADVANCED_FACE ( 'NONE', ( #19170 ), #4070, .T. ) ;
#472 = CARTESIAN_POINT ( 'NONE',  ( 43.01140435219951996, 10.71049967264875491, 34.21067981925357060 ) ) ;
#473 = CARTESIAN_POINT ( 'NONE',  ( 42.21948215057684450, 76.38361825032846752, 39.21067981925355639 ) ) ;
#474 = VECTOR ( 'NONE', #11698, 1000.000000000000114 ) ;
#475 = CARTESIAN_POINT ( 'NONE',  ( 41.64333658814960870, 146.5151871740939953, 30.00020018409699318 ) ) ;
#476 = CARTESIAN_POINT ( 'NONE',  ( 43.01140435219951286, 97.46049967264873715, 39.46799094044489209 ) ) ;
#477 = CARTESIAN_POINT ( 'NONE',  ( 20.22230697948889500, 94.36241449208007737, 1.148710122009321211 ) ) ;
#478 = FACE_OUTER_BOUND ( 'NONE', #9416, .T. ) ;
#479 = CARTESIAN_POINT ( 'NONE',  ( -141.4692556286852891, -165.8391397928654669, 46.40781461928724383 ) ) ;
#480 = FACE_OUTER_BOUND ( 'NONE', #13932, .T. ) ;
#481 = CARTESIAN_POINT ( 'NONE',  ( 63.55746018358933469, 147.2895578332197033, -9.446739241148069510 ) ) ;
#482 = CARTESIAN_POINT ( 'NONE',  ( -154.5594255724347761, -164.1630981290892919, 40.14644641866476604 ) ) ;
#483 = CARTESIAN_POINT ( 'NONE',  ( 44.37947211624943833, 80.47977050742731819, 30.00020018409699318 ) ) ;
#484 = CARTESIAN_POINT ( 'NONE',  ( -154.3824083646099439, -161.4938272943107336, 40.69124936498395328 ) ) ;
#485 = CARTESIAN_POINT ( 'NONE',  ( 43.01140435219951286, 77.36518717409400381, 29.55568802177586107 ) ) ;
#486 = DIRECTION ( 'NONE',  ( 0.000000000000000000, 1.000000000000000000, 0.000000000000000000 ) ) ;
#487 = CARTESIAN_POINT ( 'NONE',  ( 147.5268905834513475, 193.0332408774651185, 14.00000000000001776 ) ) ;
#488 = VERTEX_POINT ( 'NONE', #17503 ) ;
#489 = ADVANCED_FACE ( 'NONE', ( #5496 ), #2517, .T. ) ;
#490 = EDGE_CURVE ( 'NONE', #561, #602, #17397, .T. ) ;
#491 = CARTESIAN_POINT ( 'NONE',  ( -159.5594255724347761, -175.8630981290893089, 43.77915905869157598 ) ) ;
#492 = PLANE ( 'NONE',  #20835 ) ;
#493 = CARTESIAN_POINT ( 'NONE',  ( 39.42975644700377558, 135.6797705074273210, 36.81289934271958941 ) ) ;
#494 = CARTESIAN_POINT ( 'NONE',  ( 77.13564277734779751, 118.5067815986552375, -14.37074460762677397 ) ) ;
#495 = VERTEX_POINT ( 'NONE', #2413 ) ;
#496 = DIRECTION ( 'NONE',  ( -0.000000000000000000, 1.000000000000000000, -0.000000000000000000 ) ) ;
#497 = VERTEX_POINT ( 'NONE', #9152 ) ;
#498 = CARTESIAN_POINT ( 'NONE',  ( 46.59305225739526435, 136.5797705074272983, 36.81289934271958941 ) ) ;
#499 = CARTESIAN_POINT ( 'NONE',  ( 47.43856463449117200, 92.02977050742730114, 32.77220824515698183 ) ) ;
#500 = CARTESIAN_POINT ( 'NONE',  ( -151.4692556286852891, -181.7391397928654726, 59.65701158161631668 ) ) ;
#501 = CARTESIAN_POINT ( 'NONE',  ( 39.92123440845005433, 100.1604996726487258, 38.46393386101375711 ) ) ;
#502 = CARTESIAN_POINT ( 'NONE',  ( 43.80332655382220253, 121.9575765865522925, 29.21067981925356705 ) ) ;
#503 = CARTESIAN_POINT ( 'NONE',  ( 39.42975644700377558, 98.81518717409400665, 31.60846029578754468 ) ) ;
#504 = CARTESIAN_POINT ( 'NONE',  ( -145.6429501568359797, -155.9438272943106938, 41.63779006702063867 ) ) ;
#505 = CARTESIAN_POINT ( 'NONE',  ( 42.21948215057684450, 123.4575765865523067, 39.21067981925355639 ) ) ;
#506 = CARTESIAN_POINT ( 'NONE',  ( -161.4692556286852607, -157.4130981290893203, 52.90620854394536821 ) ) ;
#507 = CARTESIAN_POINT ( 'NONE',  ( 180.1254907973641934, 54.87273858953557237, 4.000000000000021316 ) ) ;
#508 = CARTESIAN_POINT ( 'NONE',  ( 41.46631938032478359, 146.1844580088725820, 29.45539723777780239 ) ) ;
#509 = VECTOR ( 'NONE', #17176, 1000.000000000000000 ) ;
#510 = CARTESIAN_POINT ( 'NONE',  ( 47.43856463449118621, 115.8797705074273097, 34.21067981925357060 ) ) ;
#511 =( BOUNDED_CURVE ( )  B_SPLINE_CURVE ( 2, ( #19906, #21339, #7897, #18468, #16576, #6226, #16693, #1600, #6570, #18355, #3146, #3259, #5025 ),
 .UNSPECIFIED., .F., .F. ) 
 B_SPLINE_CURVE_WITH_KNOTS ( ( 3, 2, 2, 2, 2, 2, 3 ),
 ( 0.7279411764705882026, 0.7294117647058823151, 0.7323529411764705399, 0.7352941176470588758, 0.7382352941176471006, 0.7411764705882353255, 0.7426470588235294379 ),
 .UNSPECIFIED. ) 
 CURVE ( )  GEOMETRIC_REPRESENTATION_ITEM ( )  RATIONAL_B_SPLINE_CURVE ( ( 0.9755282581475768211, 0.9755282581475768211, 1.000000000000000000, 0.9510565162951535312, 1.000000000000000000, 0.9510565162951535312, 1.000000000000000000, 0.9510565162951535312, 1.000000000000000000, 0.9510565162951535312, 1.000000000000000000, 0.9755282581475768211, 0.9755282581475768211 ) ) 
 REPRESENTATION_ITEM ( '' )  );
#512 = CARTESIAN_POINT ( 'NONE',  ( 26.48090744323847190, 142.7828511622217889, -4.776412194962503577 ) ) ;
#513 = CARTESIAN_POINT ( 'NONE',  ( 42.21948215057683740, 141.4575765865523351, 39.21067981925357060 ) ) ;
#514 = CARTESIAN_POINT ( 'NONE',  ( 44.37947211624943833, 109.0151871740940095, 38.42115945441014446 ) ) ;
#515 = ORIENTED_EDGE ( 'NONE', *, *, #14295, .T. ) ;
#516 = ADVANCED_FACE ( 'NONE', ( #17287, #19278 ), #15850, .F. ) ;
#517 = CARTESIAN_POINT ( 'NONE',  ( 159.4819454078502190, 211.3876867681337046, 14.00000000000001776 ) ) ;
#518 = CARTESIAN_POINT ( 'NONE',  ( 9.616596702810701558, 112.3753283828585694, -5.161025107254184618 ) ) ;
#519 = CARTESIAN_POINT ( 'NONE',  ( 65.09246388851926213, 137.4469437283422906, 4.918530982704383270 ) ) ;
#520 = FACE_OUTER_BOUND ( 'NONE', #589, .T. ) ;
#521 = CARTESIAN_POINT ( 'NONE',  ( 45.74753988029934249, 80.32977050742731251, 30.44471234641812174 ) ) ;
#522 = ORIENTED_EDGE ( 'NONE', *, *, #11916, .F. ) ;
#523 = CARTESIAN_POINT ( 'NONE',  ( 48.01140435219951996, 61.43445800887257491, 32.58608133808903773 ) ) ;
#524 = CARTESIAN_POINT ( 'NONE',  ( -149.8854112254399240, -165.7362167067690280, 59.65701158161632378 ) ) ;
#525 = CARTESIAN_POINT ( 'NONE',  ( 41.46631938032478359, 129.1104996726487570, 29.45539723777780239 ) ) ;
#527 = CARTESIAN_POINT ( 'NONE',  ( 42.70556344282044137, 85.75549003223034106, 1.343541076088082376 ) ) ;
#526 = CARTESIAN_POINT ( 'NONE',  ( 40.27526882409969033, 84.56518717409397823, 37.97664729208901946 ) ) ;
#528 = CARTESIAN_POINT ( 'NONE',  ( -143.8425227516148084, -183.0938272943107279, 44.11586579668791330 ) ) ;
#529 = CARTESIAN_POINT ( 'NONE',  ( -141.4692556286852891, -177.9891397928654442, 49.65701158161630957 ) ) ;
#530 = DIRECTION ( 'NONE',  ( -0.000000000000000000, 1.000000000000000000, -0.000000000000000000 ) ) ;
#531 = CARTESIAN_POINT ( 'NONE',  ( 43.01140435219950575, 140.0344580088726332, 29.21067981925357060 ) ) ;
#532 = CARTESIAN_POINT ( 'NONE',  ( 47.43856463449118621, 139.8797705074273381, 34.21067981925357060 ) ) ;
#533 = CARTESIAN_POINT ( 'NONE',  ( 47.43856463449118621, 100.8797705074273239, 34.21067981925357060 ) ) ;
#534 = CARTESIAN_POINT ( 'NONE',  ( 42.21854335081802390, 85.68333463812091111, 14.36287948008016890 ) ) ;
#535 = CARTESIAN_POINT ( 'NONE',  ( 46.59305225739526435, 133.3151871740940067, 36.81289934271958941 ) ) ;
#536 = CARTESIAN_POINT ( 'NONE',  ( -142.0420953463935803, -156.2438272943106767, 46.59394152635518793 ) ) ;
#537 = CARTESIAN_POINT ( 'NONE',  ( -142.0420953463936087, -162.6584106276440593, 49.65701158161630957 ) ) ;
#538 = DIRECTION ( 'NONE',  ( 0.000000000000000000, 0.000000000000000000, 1.000000000000000000 ) ) ;
#539 = CARTESIAN_POINT ( 'NONE',  ( 138.4989748031516967, 208.9305787985672680, -44.99999999999997158 ) ) ;
#540 = CARTESIAN_POINT ( 'NONE',  ( 15.53544334784188585, 126.6048195653137469, 15.43757839183889224 ) ) ;
#541 = CIRCLE ( 'NONE', #5131, 10.00000000000000888 ) ;
#542 = CARTESIAN_POINT ( 'NONE',  ( 39.92123440845005433, 121.1604996726487400, 38.46393386101375711 ) ) ;
#543 = CARTESIAN_POINT ( 'NONE',  ( 39.42975644700377558, 116.8151871740940067, 31.60846029578754468 ) ) ;
#544 = ORIENTED_EDGE ( 'NONE', *, *, #21756, .T. ) ;
#545 = CARTESIAN_POINT ( 'NONE',  ( -153.0531000319306543, -178.8160212151857138, 59.65701158161632378 ) ) ;
#546 = ORIENTED_EDGE ( 'NONE', *, *, #10598, .T. ) ;
#547 = CARTESIAN_POINT ( 'NONE',  ( 39.92123440845004723, 99.23445800887257917, 38.46393386101376421 ) ) ;
#548 = CARTESIAN_POINT ( 'NONE',  ( 40.27526882409969744, 146.9297705074273495, 30.44471234641812174 ) ) ;
#549 = CARTESIAN_POINT ( 'NONE',  ( 44.55648932407425633, 158.8104996726487457, 29.45539723777780239 ) ) ;
#551 = CARTESIAN_POINT ( 'NONE',  ( 63.85057544308668298, 100.9084186779620609, 13.48995955233852229 ) ) ;
#550 = CARTESIAN_POINT ( 'NONE',  ( 40.27526882409969033, 117.5651871740940067, 37.97664729208901946 ) ) ;
#552 = CARTESIAN_POINT ( 'NONE',  ( 46.10157429594899270, 76.76049967264872009, 38.46393386101376421 ) ) ;
#554 = CARTESIAN_POINT ( 'NONE',  ( 43.80332655382220253, 135.6113394311928460, 39.21067981925355639 ) ) ;
#553 = CARTESIAN_POINT ( 'NONE',  ( 43.66339603962469340, 144.9006758593374968, 29.24238570022250627 ) ) ;
#555 = CARTESIAN_POINT ( 'NONE',  ( 39.92123440845005433, 124.1604996726487400, 38.46393386101375711 ) ) ;
#556 = CARTESIAN_POINT ( 'NONE',  ( 47.56746500088171814, 95.32565373869623215, 32.14446507322556101 ) ) ;
#557 = LINE ( 'NONE', #7302, #21391 ) ;
#558 = CARTESIAN_POINT ( 'NONE',  ( -159.0959885057557983, -176.1938272943107506, 44.11586579668791330 ) ) ;
#559 = FACE_OUTER_BOUND ( 'NONE', #21629, .T. ) ;
#560 = AXIS2_PLACEMENT_3D ( 'NONE', #8557, #13714, #11956 ) ;
#561 = VERTEX_POINT ( 'NONE', #8931 ) ;
#562 = CARTESIAN_POINT ( 'NONE',  ( -160.8964159109769696, -176.3084106276440082, 46.59394152635518793 ) ) ;
#563 = CARTESIAN_POINT ( 'NONE',  ( 26.28242620001017471, 89.94675250444232972, 6.906269859504051922 ) ) ;
#564 = CYLINDRICAL_SURFACE ( 'NONE', #18674, 10.00000000000000888 ) ;
#565 = CARTESIAN_POINT ( 'NONE',  ( 45.74753988029933538, 142.1651871740940010, 37.97664729208901946 ) ) ;
#566 = ADVANCED_FACE ( 'NONE', ( #7498 ), #12330, .F. ) ;
#567 = CARTESIAN_POINT ( 'NONE',  ( -81.61981105773979550, 604.5992151483073940, -0.8325491102011938205 ) ) ;
#568 = CARTESIAN_POINT ( 'NONE',  ( 38.58424406990786082, 108.3797705074273239, 34.21067981925357060 ) ) ;
#569 = CARTESIAN_POINT ( 'NONE',  ( 74.85601106972485752, 107.3429126181175661, -0.9942341299615756745 ) ) ;
#570 = ORIENTED_EDGE ( 'NONE', *, *, #6351, .T. ) ;
#571 = CARTESIAN_POINT ( 'NONE',  ( 32.47916914626341622, 146.0660553311768979, 3.489959554161691013 ) ) ;
#572 = AXIS2_PLACEMENT_3D ( 'NONE', #18716, #10458, #2366 ) ;
#573 = ORIENTED_EDGE ( 'NONE', *, *, #1822, .T. ) ;
#574 = CARTESIAN_POINT ( 'NONE',  ( 39.42975644700377558, 111.6797705074273210, 36.81289934271958941 ) ) ;
#575 = CARTESIAN_POINT ( 'NONE',  ( 39.92123440845005433, 131.3344580088725593, 29.95742577749336988 ) ) ;
#576 = CARTESIAN_POINT ( 'NONE',  ( 46.10157429594899270, 88.76049967264872009, 38.46393386101375711 ) ) ;
#577 = CARTESIAN_POINT ( 'NONE',  ( 40.27526882409969033, 81.82977050742729830, 37.97664729208901946 ) ) ;
#578 = CARTESIAN_POINT ( 'NONE',  ( 44.37947211624943833, 146.2151871740940123, 30.00020018409699318 ) ) ;
#579 = CARTESIAN_POINT ( 'NONE',  ( 48.01140435219951996, 101.2104996726487514, 34.21067981925357060 ) ) ;
#580 = CARTESIAN_POINT ( 'NONE',  ( 51.60797029699607918, 86.77139250312444574, -6.946567135388369785 ) ) ;
#581 = CARTESIAN_POINT ( 'NONE',  ( 41.46631938032478359, 60.11049967264874283, 29.45539723777780239 ) ) ;
#582 = CARTESIAN_POINT ( 'NONE',  ( -141.4692556286852891, -168.9891397928654726, 49.65701158161630957 ) ) ;
#583 = VECTOR ( 'NONE', #3604, 1000.000000000000114 ) ;
#584 = CARTESIAN_POINT ( 'NONE',  ( -145.2889157411863437, -158.6130981290893089, 41.15050349809589392 ) ) ;
#585 = CARTESIAN_POINT ( 'NONE',  ( 38.96631938032478359, 143.4844580088725650, 31.27175355779120025 ) ) ;
#586 = ADVANCED_BREP_SHAPE_REPRESENTATION ( '', ( #14581, #283, #12657 ), #11603 ) ;
#587 = CARTESIAN_POINT ( 'NONE',  ( 48.01140435219951996, 106.1344580088725849, 35.83527830041809636 ) ) ;
#588 = EDGE_CURVE ( 'NONE', #6094, #10912, #2565, .T. ) ;
#589 = EDGE_LOOP ( 'NONE', ( #10743, #2541, #5246, #20217, #1667 ) ) ;
#590 = AXIS2_PLACEMENT_3D ( 'NONE', #17670, #14043, #3917 ) ;
#591 = CARTESIAN_POINT ( 'NONE',  ( 38.58424406990784661, 81.22977050742731819, 32.77220824515698183 ) ) ;
#592 = CARTESIAN_POINT ( 'NONE',  ( -151.4692556286852891, -167.6438272943107108, 39.74470866294723947 ) ) ;
#593 = EDGE_CURVE ( 'NONE', #21705, #4967, #4602, .T. ) ;
#594 = CARTESIAN_POINT ( 'NONE',  ( 46.59305225739526435, 82.91518717409400097, 31.60846029578754468 ) ) ;
#595 = FACE_OUTER_BOUND ( 'NONE', #8168, .T. ) ;
#596 = ORIENTED_EDGE ( 'NONE', *, *, #1004, .F. ) ;
#597 = CARTESIAN_POINT ( 'NONE',  ( 38.96631938032478359, 117.4104996726487400, 31.27175355779120025 ) ) ;
#598 = CARTESIAN_POINT ( 'NONE',  ( 147.5268905834513475, 193.0332408774651185, 14.00000000000001776 ) ) ;
#599 = CARTESIAN_POINT ( 'NONE',  ( 45.74753988029934249, 133.4297705074273210, 37.97664729208901235 ) ) ;
#600 = CARTESIAN_POINT ( 'NONE',  ( 19.41497643977705323, 135.2012136132025546, 3.803670830490076149 ) ) ;
#601 = EDGE_CURVE ( 'NONE', #16938, #20322, #15854, .T. ) ;
#602 = VERTEX_POINT ( 'NONE', #3063 ) ;
#603 = CYLINDRICAL_SURFACE ( 'NONE', #15728, 10.00000000000000888 ) ;
#604 = ORIENTED_EDGE ( 'NONE', *, *, #3541, .T. ) ;
#605 = VECTOR ( 'NONE', #15968, 1000.000000000000000 ) ;
#606 = CARTESIAN_POINT ( 'NONE',  ( 38.58424406990784661, 138.2297705074273324, 32.77220824515698183 ) ) ;
#607 = CARTESIAN_POINT ( 'NONE',  ( 47.43856463449118621, 91.87977050742732388, 34.21067981925357060 ) ) ;
#608 = ADVANCED_FACE ( 'NONE', ( #12767 ), #11547, .T. ) ;
#609 = LINE ( 'NONE', #7345, #1308 ) ;
#610 = CARTESIAN_POINT ( 'NONE',  ( 39.92123440845005433, 130.1604996726487684, 38.46393386101375711 ) ) ;
#611 = CARTESIAN_POINT ( 'NONE',  ( -145.2889157411863437, -194.6130981290892805, 41.15050349809589392 ) ) ;
#612 = VECTOR ( 'NONE', #11258, 1000.000000000000227 ) ;
#613 = CARTESIAN_POINT ( 'NONE',  ( 46.59305225739526435, 94.31518717409399244, 36.81289934271958941 ) ) ;
#614 = CARTESIAN_POINT ( 'NONE',  ( 43.01140435219951286, 124.4604996726487371, 39.21067981925356349 ) ) ;
#615 = CARTESIAN_POINT ( 'NONE',  ( -157.6495955161842062, -164.0130981290892862, 41.15050349809590102 ) ) ;
#616 = DIRECTION ( 'NONE',  ( 0.000000000000000000, 0.000000000000000000, 1.000000000000000000 ) ) ;
#617 = CARTESIAN_POINT ( 'NONE',  ( 47.05648932407426344, 108.9844580088725792, 37.14960608071593384 ) ) ;
#618 = EDGE_CURVE ( 'NONE', #16530, #3067, #6233, .T. ) ;
#619 = CARTESIAN_POINT ( 'NONE',  ( 44.55648932407425633, 129.6844580088725820, 38.96596240072933170 ) ) ;
#620 = CARTESIAN_POINT ( 'NONE',  ( 39.42975644700377558, 114.6797705074273210, 36.81289934271958941 ) ) ;
#621 = CARTESIAN_POINT ( 'NONE',  ( 54.90439719837324617, 94.24896709312837118, 12.93774216356182372 ) ) ;
#622 = CARTESIAN_POINT ( 'NONE',  ( -145.6429501568359797, -192.8438272943107563, 57.67623309621198047 ) ) ;
#623 = CARTESIAN_POINT ( 'NONE',  ( 40.27526882409969744, 104.6651871740940010, 30.44471234641812174 ) ) ;
#624 = AXIS2_PLACEMENT_3D ( 'NONE', #1762, #13223, #18408 ) ;
#625 = EDGE_LOOP ( 'NONE', ( #14044, #7065, #9180, #16970 ) ) ;
#626 = CARTESIAN_POINT ( 'NONE',  ( 42.21948215057684450, 87.03738109496902098, 29.21067981925356705 ) ) ;
#627 = CARTESIAN_POINT ( 'NONE',  ( 26.87026879109711786, 150.0197496251087728, 11.30891725959585159 ) ) ;
#628 = CARTESIAN_POINT ( 'NONE',  ( 68.77576173894735234, 108.4446202281264249, 13.13264940013829296 ) ) ;
#629 = CYLINDRICAL_SURFACE ( 'NONE', #11092, 4.999999999999997335 ) ;
#630 = CARTESIAN_POINT ( 'NONE',  ( 43.01140435219951286, 73.12977050742730967, 38.86567161673127657 ) ) ;
#631 = ORIENTED_EDGE ( 'NONE', *, *, #10728, .F. ) ;
#632 = VECTOR ( 'NONE', #4152, 1000.000000000000227 ) ;
#633 = CIRCLE ( 'NONE', #13999, 7.500000000000000000 ) ;
#634 = CARTESIAN_POINT ( 'NONE',  ( 48.01140435219951996, 61.13445800887257775, 35.83527830041810347 ) ) ;
#635 = CARTESIAN_POINT ( 'NONE',  ( -145.2889157411863437, -171.5391397928654555, 41.15050349809589392 ) ) ;
#636 = COLOUR_RGB ( '', 0.72549020, 0.75294118, 0.79215686) ;
#637 = CARTESIAN_POINT ( 'NONE',  ( 44.55648932407425633, 116.8104996726487599, 29.45539723777780239 ) ) ;
#639 = CARTESIAN_POINT ( 'NONE',  ( 41.12929731208597417, 154.0090796829547912, -2.227802639778228233 ) ) ;
#638 = CARTESIAN_POINT ( 'NONE',  ( 44.37947211624943833, 74.21518717409399812, 30.00020018409699318 ) ) ;
#640 =( BOUNDED_CURVE ( )  B_SPLINE_CURVE ( 2, ( #17679, #2582, #18348, #21774, #1486, #18236, #11620, #1154, #16245, #3251, #11392, #16459, #13390 ),
 .UNSPECIFIED., .F., .F. ) 
 B_SPLINE_CURVE_WITH_KNOTS ( ( 3, 2, 2, 2, 2, 2, 3 ),
 ( 0.6691176470588234837, 0.6705882352941175961, 0.6735294117647059320, 0.6764705882352941568, 0.6794117647058823817, 0.6823529411764706065, 0.6838235294117647189 ),
 .UNSPECIFIED. ) 
 CURVE ( )  GEOMETRIC_REPRESENTATION_ITEM ( )  RATIONAL_B_SPLINE_CURVE ( ( 0.9755282581475768211, 0.9755282581475768211, 1.000000000000000000, 0.9510565162951535312, 1.000000000000000000, 0.9510565162951535312, 1.000000000000000000, 0.9510565162951535312, 1.000000000000000000, 0.9510565162951535312, 1.000000000000000000, 0.9755282581475768211, 0.9755282581475768211 ) ) 
 REPRESENTATION_ITEM ( '' )  );
#641 = CARTESIAN_POINT ( 'NONE',  ( -159.0959885057557983, -179.1938272943107506, 44.11586579668791330 ) ) ;
#642 = CARTESIAN_POINT ( 'NONE',  ( 47.05648932407426344, 113.5104996726487485, 31.27175355779120025 ) ) ;
#643 = CARTESIAN_POINT ( 'NONE',  ( -141.4692556286852891, -186.2130981290892748, 52.90620854394536821 ) ) ;
#644 = FACE_OUTER_BOUND ( 'NONE', #12393, .T. ) ;
#645 = CARTESIAN_POINT ( 'NONE',  ( 39.92123440845004723, 158.3344580088725877, 29.95742577749337343 ) ) ;
#646 = CARTESIAN_POINT ( 'NONE',  ( 44.37947211624943833, 142.2797705074273154, 38.42115945441014446 ) ) ;
#647 = CARTESIAN_POINT ( 'NONE',  ( 43.01140435219951286, 107.6297705074272955, 29.55568802177586463 ) ) ;
#648 = CARTESIAN_POINT ( 'NONE',  ( 9.231363607564425422, 125.4582397780895633, 16.26765482522027639 ) ) ;
#649 = CARTESIAN_POINT ( 'NONE',  ( 40.27526882409969744, 132.5651871740939782, 37.97664729208901235 ) ) ;
#650 = CARTESIAN_POINT ( 'NONE',  ( -145.6429501568359797, -156.8438272943107563, 57.67623309621198047 ) ) ;
#651 = CARTESIAN_POINT ( 'NONE',  ( -157.2955611005345986, -169.7084106276440139, 57.67623309621197336 ) ) ;
#652 = CARTESIAN_POINT ( 'NONE',  ( -153.0531000319307111, -163.8160212151857706, 59.65701158161632378 ) ) ;
#653 = FACE_OUTER_BOUND ( 'NONE', #17209, .T. ) ;
#654 = CARTESIAN_POINT ( 'NONE',  ( 46.21245884545565019, 91.80782910428004584, 13.29499484581607582 ) ) ;
#655 = CARTESIAN_POINT ( 'NONE',  ( 47.43856463449117200, 118.7651871740940237, 32.77220824515698183 ) ) ;
#656 = ORIENTED_EDGE ( 'NONE', *, *, #19082, .T. ) ;
#657 = DIRECTION ( 'NONE',  ( 0.000000000000000000, 0.000000000000000000, 1.000000000000000000 ) ) ;
#658 = ORIENTED_EDGE ( 'NONE', *, *, #12587, .F. ) ;
#659 = CARTESIAN_POINT ( 'NONE',  ( 38.96631938032478359, 95.48445800887257917, 31.27175355779120025 ) ) ;
#660 = EDGE_CURVE ( 'NONE', #15106, #2386, #14957, .T. ) ;
#661 = EDGE_CURVE ( 'NONE', #393, #1664, #4822, .T. ) ;
#662 = CARTESIAN_POINT ( 'NONE',  ( 38.96631938032478359, 157.0104996726487343, 37.14960608071593384 ) ) ;
#664 = CARTESIAN_POINT ( 'NONE',  ( 55.97020510223934764, 144.8627979930266463, -1.553355716038981038 ) ) ;
#663 = CARTESIAN_POINT ( 'NONE',  ( 47.43856463449117200, 103.4651871740939839, 35.64915139335016647 ) ) ;
#665 = CARTESIAN_POINT ( 'NONE',  ( 43.01140435219951286, 76.46049967264872294, 39.46799094044489209 ) ) ;
#667 = CARTESIAN_POINT ( 'NONE',  ( -159.5594255724347761, -157.8630981290893089, 43.77915905869157598 ) ) ;
#666 = CARTESIAN_POINT ( 'NONE',  ( -151.4692556286852891, -196.9891397928655010, 49.65701158161630957 ) ) ;
#668 = AXIS2_PLACEMENT_3D ( 'NONE', #14423, #4498, #6045 ) ;
#669 = CARTESIAN_POINT ( 'NONE',  ( -159.5594255724347761, -172.2630981290892862, 55.53486410454104316 ) ) ;
#670 = CARTESIAN_POINT ( 'NONE',  ( 111.4021762516569964, 137.5714195593754710, -19.99999999999997868 ) ) ;
#671 = CARTESIAN_POINT ( 'NONE',  ( 39.42975644700377558, 68.81518717409400665, 31.60846029578754468 ) ) ;
#672 = LINE ( 'NONE', #7408, #19081 ) ;
#673 = CARTESIAN_POINT ( 'NONE',  ( -143.8425227516148084, -180.6938272943107506, 55.19815736654470584 ) ) ;
#674 = CARTESIAN_POINT ( 'NONE',  ( -142.0420953463935803, -189.8084106276440366, 52.72008163687743831 ) ) ;
#675 = EDGE_LOOP ( 'NONE', ( #12068, #12531, #7663, #2302 ) ) ;
#676 = CARTESIAN_POINT ( 'NONE',  ( 13.60337824163328513, 137.5875211305428252, 8.692014997358331385 ) ) ;
#677 = ADVANCED_FACE ( 'NONE', ( #16611 ), #4491, .T. ) ;
#678 = CARTESIAN_POINT ( 'NONE',  ( 147.8787791192428074, -126.9891397928655010, 49.65701158161629536 ) ) ;
#679 = CARTESIAN_POINT ( 'NONE',  ( 47.43856463449117200, 148.4651871740940123, 35.64915139335016647 ) ) ;
#680 = CARTESIAN_POINT ( 'NONE',  ( 38.58424406990786082, 156.1151871740940180, 34.21067981925357060 ) ) ;
#681 = CARTESIAN_POINT ( 'NONE',  ( 47.43856463449118621, 109.8797705074273239, 34.21067981925357060 ) ) ;
#682 = ORIENTED_EDGE ( 'NONE', *, *, #18825, .F. ) ;
#683 = ORIENTED_EDGE ( 'NONE', *, *, #21000, .F. ) ;
#684 = VECTOR ( 'NONE', #722, 1000.000000000000000 ) ;
#685 = CARTESIAN_POINT ( 'NONE',  ( 70.03002323795641360, 111.8333997399938511, 5.989792257250448060 ) ) ;
#686 = ORIENTED_EDGE ( 'NONE', *, *, #10694, .T. ) ;
#687 = CARTESIAN_POINT ( 'NONE',  ( 48.01140435219951996, 118.2844580088725763, 34.21067981925357060 ) ) ;
#688 = CARTESIAN_POINT ( 'NONE',  ( 47.05648932407426344, 88.91049967264873999, 37.14960608071593384 ) ) ;
#689 = CARTESIAN_POINT ( 'NONE',  ( 38.58424406990786082, 147.1151871740939896, 34.21067981925357060 ) ) ;
#690 = CARTESIAN_POINT ( 'NONE',  ( 46.10157429594899270, 97.76049967264872009, 38.46393386101376421 ) ) ;
#691 = CARTESIAN_POINT ( 'NONE',  ( 61.61057083318216598, 91.16763906547615193, -7.303593892219363504 ) ) ;
#692 = DIRECTION ( 'NONE',  ( -1.000000000000000000, 0.000000000000000000, 0.000000000000000000 ) ) ;
#693 = EDGE_CURVE ( 'NONE', #7475, #16674, #7926, .T. ) ;
#694 = CARTESIAN_POINT ( 'NONE',  ( -157.6495955161842062, -167.0391397928654271, 58.16351966513671812 ) ) ;
#695 = CARTESIAN_POINT ( 'NONE',  ( 43.01140435219951996, 158.9604996726487514, 29.21067981925357060 ) ) ;
#696 = DIRECTION ( 'NONE',  ( 0.9999746145782334450, -0.007125320983191549967, 0.000000000000000000 ) ) ;
#697 =( REPRESENTATION_RELATIONSHIP ('NONE','NONE', #6933, #8609 ) REPRESENTATION_RELATIONSHIP_WITH_TRANSFORMATION ( #1489 )SHAPE_REPRESENTATION_RELATIONSHIP( ) );
#698 = CARTESIAN_POINT ( 'NONE',  ( 47.43856463449118621, 148.6151871740939896, 34.21067981925357060 ) ) ;
#699 = ORIENTED_EDGE ( 'NONE', *, *, #16016, .T. ) ;
#700 = CARTESIAN_POINT ( 'NONE',  ( 47.43856463449118621, 82.87977050742730967, 34.21067981925357060 ) ) ;
#701 = CARTESIAN_POINT ( 'NONE',  ( -142.0420953463936087, -162.3938272943107393, 49.65701158161630957 ) ) ;
#702 = CARTESIAN_POINT ( 'NONE',  ( 45.74753988029934249, 67.16518717409400097, 37.97664729208901235 ) ) ;
#703 = CARTESIAN_POINT ( 'NONE',  ( 69.71972837475884432, 98.49221204361529658, -7.660766391518695428 ) ) ;
#704 = PRODUCT_RELATED_PRODUCT_CATEGORY ( 'part', '', ( #14993 ) ) ;
#705 = CARTESIAN_POINT ( 'NONE',  ( -142.0420953463935803, -192.8084106276440650, 52.72008163687743831 ) ) ;
#706 = VERTEX_POINT ( 'NONE', #21264 ) ;
#707 = FACE_OUTER_BOUND ( 'NONE', #3120, .T. ) ;
#708 = CARTESIAN_POINT ( 'NONE',  ( 41.46631938032478359, 105.3844580088725849, 38.96596240072933170 ) ) ;
#709 = CARTESIAN_POINT ( 'NONE',  ( 46.59305225739526435, 137.1797705074273210, 31.60846029578754468 ) ) ;
#710 = CARTESIAN_POINT ( 'NONE',  ( 43.31828379119179573, 154.0590585871367750, -16.15632009132952973 ) ) ;
#711 = VERTEX_POINT ( 'NONE', #6143 ) ;
#712 = EDGE_CURVE ( 'NONE', #6431, #3596, #14744, .T. ) ;
#713 = CARTESIAN_POINT ( 'NONE',  ( 43.01140435219953417, 140.9604996726487514, 29.21067981925357060 ) ) ;
#714 = ORIENTED_EDGE ( 'NONE', *, *, #4516, .T. ) ;
#715 = CARTESIAN_POINT ( 'NONE',  ( 43.01140435219951286, 139.1297705074272812, 38.86567161673127657 ) ) ;
#716 = CARTESIAN_POINT ( 'NONE',  ( 47.05648932407426344, 133.9104996726487400, 37.14960608071593384 ) ) ;
#717 = CARTESIAN_POINT ( 'NONE',  ( 38.58424406990786082, 93.37977050742732388, 34.21067981925357060 ) ) ;
#719 = EDGE_CURVE ( 'NONE', #19361, #7226, #16390, .T. ) ;
#718 = CARTESIAN_POINT ( 'NONE',  ( 48.01140435219951996, 155.2104996726487514, 34.21067981925357060 ) ) ;
#720 = DIRECTION ( 'NONE',  ( 1.000000000000000000, 0.000000000000000000, 0.000000000000000000 ) ) ;
#721 = CARTESIAN_POINT ( 'NONE',  ( 43.01140435219951286, 120.5344580088725763, 39.21067981925356349 ) ) ;
#722 = DIRECTION ( 'NONE',  ( 0.000000000000000000, 0.000000000000000000, 1.000000000000000000 ) ) ;
#723 = CARTESIAN_POINT ( 'NONE',  ( 47.43856463449117200, 100.7651871740939953, 32.77220824515698183 ) ) ;
#724 = CYLINDRICAL_SURFACE ( 'NONE', #15405, 7.500000000000007105 ) ;
#725 = CARTESIAN_POINT ( 'NONE',  ( 43.01140435219951286, 125.9604996726487514, 29.21067981925356705 ) ) ;
#726 = CARTESIAN_POINT ( 'NONE',  ( -151.4692556286852891, -161.3130981290892692, 39.14238933923362396 ) ) ;
#727 = APPLICATION_PROTOCOL_DEFINITION ( 'draft international standard', 'automotive_design', 1998, #7051 ) ;
#728 = CARTESIAN_POINT ( 'NONE',  ( 48.01140435219951996, 71.36049967264874283, 32.58608133808903773 ) ) ;
#729 = CARTESIAN_POINT ( 'NONE',  ( 46.10157429594899270, 136.7344580088725365, 29.95742577749337343 ) ) ;
#730 = CARTESIAN_POINT ( 'NONE',  ( 40.27526882409969033, 116.9297705074273210, 30.44471234641811819 ) ) ;
#731 = CARTESIAN_POINT ( 'NONE',  ( 18.61283035262889385, 105.6058852300018032, 7.580709131559767222 ) ) ;
#732 = CARTESIAN_POINT ( 'NONE',  ( -145.6429501568359797, -189.8438272943106995, 57.67623309621198047 ) ) ;
#733 = CARTESIAN_POINT ( 'NONE',  ( 39.42975644700377558, 95.81518717409399244, 31.60846029578754468 ) ) ;
#734 = CARTESIAN_POINT ( 'NONE',  ( 43.01140435219951286, 91.46049967264873715, 39.21067981925356349 ) ) ;
#735 = VERTEX_POINT ( 'NONE', #15411 ) ;
#736 = VECTOR ( 'NONE', #19488, 1000.000000000000000 ) ;
#737 = CARTESIAN_POINT ( 'NONE',  ( 39.92123440845005433, 87.26049967264874851, 29.95742577749336988 ) ) ;
#738 = CARTESIAN_POINT ( 'NONE',  ( 38.34086628137072239, 86.07498427433979771, 8.486398261126511855 ) ) ;
#739 = CARTESIAN_POINT ( 'NONE',  ( 16.97565887011968400, 109.0741130153051444, 8.727962422049884594 ) ) ;
#740 = CARTESIAN_POINT ( 'NONE',  ( 46.59305225739526435, 80.17977050742732104, 31.60846029578754468 ) ) ;
#741 = ORIENTED_EDGE ( 'NONE', *, *, #12992, .T. ) ;
#742 = EDGE_LOOP ( 'NONE', ( #2278, #4882, #741, #4097, #12117, #6348, #5852, #596 ) ) ;
#743 = CARTESIAN_POINT ( 'NONE',  ( 157.5268905834513475, 193.0332408774651185, -50.99999999999998579 ) ) ;
#744 = CARTESIAN_POINT ( 'NONE',  ( 46.10157429594899270, 115.7604996726487343, 38.46393386101376421 ) ) ;
#746 = CARTESIAN_POINT ( 'NONE',  ( 31.96084264191244273, 87.59053552682176758, 1.700516636338098797 ) ) ;
#745 = CARTESIAN_POINT ( 'NONE',  ( 45.74753988029933538, 76.16518717409400097, 37.97664729208901946 ) ) ;
#747 = CARTESIAN_POINT ( 'NONE',  ( -145.6429501568359797, -174.8438272943107279, 57.67623309621197336 ) ) ;
#748 = CARTESIAN_POINT ( 'NONE',  ( 43.01140435219951286, 112.4604996726487514, 39.21067981925356349 ) ) ;
#749 = CARTESIAN_POINT ( 'NONE',  ( -151.4692556286852891, -188.3130981290892407, 39.14238933923362396 ) ) ;
#750 = CARTESIAN_POINT ( 'NONE',  ( 38.01140435219952707, 80.78445800887257633, 34.21067981925357060 ) ) ;
#751 = DIRECTION ( 'NONE',  ( 1.000000000000000000, 0.000000000000000000, 0.000000000000000000 ) ) ;
#752 = CARTESIAN_POINT ( 'NONE',  ( 41.46631938032478359, 150.3844580088725991, 38.96596240072933170 ) ) ;
#753 = CARTESIAN_POINT ( 'NONE',  ( 47.43856463449117200, 143.0297705074273154, 32.77220824515698183 ) ) ;
#754 = CARTESIAN_POINT ( 'NONE',  ( 29.59780345622613851, 88.32329120701308511, 6.787350155335245994 ) ) ;
#755 = CARTESIAN_POINT ( 'NONE',  ( 40.27526882409969744, 140.6651871740939725, 30.44471234641812174 ) ) ;
#756 = CARTESIAN_POINT ( 'NONE',  ( 38.96631938032478359, 70.01049967264874851, 37.14960608071593384 ) ) ;
#757 = CARTESIAN_POINT ( 'NONE',  ( -160.8964159109769696, -164.0084106276440536, 52.72008163687743121 ) ) ;
#758 = DIRECTION ( 'NONE',  ( 1.000000000000000000, 0.000000000000000000, 0.000000000000000000 ) ) ;
#759 = CARTESIAN_POINT ( 'NONE',  ( -151.4692556286852891, -196.9891397928655010, 59.65701158161632378 ) ) ;
#760 = CARTESIAN_POINT ( 'NONE',  ( 70.16915148685765757, 112.0176666281686977, 11.98539833154344691 ) ) ;
#761 = CARTESIAN_POINT ( 'NONE',  ( 0.000000000000000000, -126.9891397928655010, 0.000000000000000000 ) ) ;
#762 = CARTESIAN_POINT ( 'NONE',  ( 45.74753988029933538, 103.1651871740940010, 37.97664729208901946 ) ) ;
#763 = ADVANCED_FACE ( 'NONE', ( #12088 ), #11983, .F. ) ;
#764 = EDGE_LOOP ( 'NONE', ( #17589, #5670, #19623, #11053, #11158, #714, #21133, #1352, #4663, #16860, #12738, #15157, #16180, #21181, #544, #656, #18743, #2229, #14338, #3756, #14681, #12360, #12066, #4072, #7203, #7344, #13067, #15491, #10510, #14069, #9237 ) ) ;
#765 = CARTESIAN_POINT ( 'NONE',  ( 136.0032066456581390, 182.5367998656340944, 34.00000000000001421 ) ) ;
#766 = ORIENTED_EDGE ( 'NONE', *, *, #1366, .T. ) ;
#767 =( BOUNDED_SURFACE ( )  B_SPLINE_SURFACE ( 1, 2, ( 
 ( #3931, #20794, #12409, #11076, #941, #7787, #10878, #14491, #2382, #21233, #6112, #10766, #14383, #7686, #12735, #9329, #10662, #622, #19458, #17364, #9007, #17791, #17687, #19140, #2485, #2699, #9227, #9444, #2270, #15718, #7357, #15925, #837, #14060, #5686, #9120, #4039, #732, #15818, #7460, #7571, #14271, #21016, #4248, #5898, #19350, #10974, #2589, #21673, #6450, #6568, #8331, #9550, #16253, #3257, #13288, #2812, #11513, #20023, #15040, #16574, #4909, #18013, #14597, #18242, #1162, #4570, #4455, #2924, #17899, #3144, #21337, #1598, #13172, #9987, #16690, #9874, #12955, #9769, #21781, #11186, #19904, #8005, #12842, #19560, #3032, #18353, #14924, #14712, #4792, #7895, #6224, #21448, #16466, #19678, #6338, #9659, #16359, #1493, #1270, #13064, #19791, #4683, #14815, #11398, #1380, #21560, #18122, #8109, #8223, #2035, #8767, #17225, #5440, #1821, #15153, #11732, #12056, #3585, #15482, #18892, #20447, #15380, #383, #20129, #13395, #7112, #8555, #13604, #10527, #20557, #12160, #3799, #10313, #15581, #10206, #15267, #18787, #11846, #5339, #54, #18575, #164, #2141, #13817, #8874, #3482, #273, #6687, #17015, #5236, #1922, #6796, #3368, #16800, #20341, #16909, #5023, #17123, #3690, #11953, #18465, #10093, #18683, #10418, #1713, #8658, #6897, #8448, #7007, #13503, #20235, #5128, #13711, #914, #15896, #4325, #12602, #19324, #2245, #20987, #15685, #17441, #7435, #2458, #592, #7332, #14032, #19431, #9089, #20767, #14357, #12491, #20662, #7221, #14138, #9198, #2352, #12381, #7660, #2669, #8979, #5981, #5658, #4223, #19116, #12707, #20875, #9303, #21098, #5763, #11050, #3908, #13922, #19006, #17765, #808, #15792, #4116, #10952, #701, #19218, #7545, #17660, #4011, #9413, #484, #2566, #5543, #10852, #12270, #10739, #17548, #17338, #4762, #19763, #1465, #17873, #16121, #6196, #4543, #19652, #3227, #21311, #19875, #14461, #1027, #1354, #6087, #8197, #14898, #13146, #3117, #9743, #9848, #11598, #12815, #19534, #6537, #16549, #4428, #14792, #21646, #18328, #11481, #13257, #12927, #2784, #21534 ),
 ( #16440, #19994, #4879, #18212, #16224, #13039, #7764, #21203, #8085, #11265, #11160, #9527, #6312, #1135, #7869, #17984, #6424, #14569, #2898, #9633, #4660, #16332, #1242, #7976, #14683, #21423, #11375, #18096, #3005, #1797, #11926, #16775, #139, #18655, #15010, #10067, #16988, #5316, #12029, #20529, #3559, #7086, #13368, #11704, #17094, #3456, #5102, #20313, #10283, #18763, #13789, #16664, #3664, #10394, #29, #1575, #18440, #3339, #2008, #6982, #5415, #11818, #12133, #8416, #18866, #9961, #1686, #8741, #13685, #15458, #243, #8303, #20105, #358, #21751, #6660, #20419, #8631, #15125, #8528, #4994, #15241, #6767, #13476, #20208, #18549, #6869, #13577, #10179, #16880, #5212, #1895, #15349, #12464, #14332, #7193, #5517, #10927, #19090, #20741, #14112, #4092, #20961, #21073, #10502, #12575, #5846, #15659, #2114, #18978, #3881, #17634, #7520, #5955, #12354, #3773, #2222, #8851, #461, #17310, #2542, #14221, #9279, #15872, #13897, #20636, #15980, #10606, #8953, #562, #7307, #14007, #17418, #3990, #2324, #10715, #9062, #7413, #20850, #19195, #10824, #17524, #14768, #2762, #8170, #1111, #6511, #9502, #1327, #17740, #19404, #4629, #9387, #4737, #11456, #16417, #6396, #13016, #13124, #14875, #16092, #1002, #9825, #19846, #7739, #18071, #18185, #21620, #8060, #3092, #16199, #21174, #2978, #14440, #11136, #11027, #7846, #2645, #9716, #6065, #4301, #19736, #16523, #1441, #21511, #19512, #16308, #12792, #4404, #11348, #14548, #17851, #21291, #9610, #6169, #12903, #19625, #4519, #11241, #17961, #2866, #1219, #7952, #14657, #21397, #6285, #1769, #4969, #8604, #13345, #4, #18523, #6632, #13453, #3432, #11573, #14982, #16855, #20289, #5183, #8281, #18302, #15216, #20187, #11902, #15325, #8503, #10154, #18631, #19969, #4853, #3535, #16749, #15100, #218, #10260, #1874, #16962, #5079, #20395, #18418, #10045, #115, #20082, #6846, #21727, #11681, #1658, #6954, #13661, #13231, #8391, #13554, #3204, #9935, #16640, #1550, #11793, #6745, #3316, #18032, #1177, #13187, #21575, #8127, #9675, #1073, #6586, #2938 ) ),
 .UNSPECIFIED., .F., .F., .F. ) 
 B_SPLINE_SURFACE_WITH_KNOTS ( ( 2, 2 ),
 ( 3, 2, 2, 2, 2, 2, 2, 2, 2, 2, 2, 2, 2, 2, 2, 2, 2, 2, 2, 2, 2, 2, 2, 2, 2, 2, 2, 2, 2, 2, 2, 2, 2, 2, 2, 2, 2, 2, 2, 2, 2, 2, 2, 2, 2, 2, 2, 2, 2, 2, 2, 2, 2, 2, 2, 2, 2, 2, 2, 2, 2, 2, 2, 2, 2, 2, 2, 2, 2, 2, 2, 2, 2, 2, 2, 2, 2, 2, 2, 2, 2, 2, 2, 2, 2, 2, 2, 2, 2, 2, 2, 2, 2, 2, 2, 2, 2, 2, 2, 2, 2, 2, 2, 2, 2, 2, 2, 2, 2, 2, 2, 2, 2, 2, 2, 2, 2, 2, 2, 2, 2, 2, 2, 2, 2, 2, 2, 2, 2, 2, 2, 2, 2, 2, 3 ),
 ( 0.000000000000000000, 1.000000000000000000 ),
 ( 0.000000000000000000, 0.007142857142857142634, 0.01428571428571428527, 0.02142857142857142877, 0.02857142857142857054, 0.03571428571428571230, 0.04285714285714285754, 0.05000000000000000278, 0.05714285714285714107, 0.06428571428571427937, 0.07142857142857142461, 0.07857142857142856984, 0.08571428571428571508, 0.09285714285714286031, 0.1000000000000000056, 0.1071428571428571369, 0.1142857142857142821, 0.1214285714285714274, 0.1285714285714285587, 0.1357142857142857040, 0.1428571428571428492, 0.1499999999999999944, 0.1571428571428571397, 0.1642857142857142849, 0.1714285714285714302, 0.1785714285714285754, 0.1857142857142857206, 0.1928571428571428659, 0.2000000000000000111, 0.2071428571428571563, 0.2142857142857142738, 0.2214285714285714191, 0.2285714285714285643, 0.2357142857142857095, 0.2428571428571428548, 0.2500000000000000000, 0.2571428571428571175, 0.2642857142857142905, 0.2714285714285714080, 0.2785714285714285809, 0.2857142857142856984, 0.2928571428571428714, 0.2999999999999999889, 0.3071428571428571619, 0.3142857142857142794, 0.3214285714285714524, 0.3285714285714285698, 0.3357142857142856873, 0.3428571428571428603, 0.3499999999999999778, 0.3571428571428571508, 0.3642857142857142683, 0.3714285714285714413, 0.3785714285714285587, 0.3857142857142857317, 0.3928571428571428492, 0.4000000000000000222, 0.4071428571428571397, 0.4142857142857143127, 0.4214285714285714302, 0.4285714285714285476, 0.4357142857142857206, 0.4428571428571428381, 0.4500000000000000111, 0.4571428571428571286, 0.4642857142857143016, 0.4714285714285714191, 0.4785714285714285920, 0.4857142857142857095, 0.4928571428571428825, 0.5000000000000000000, 0.5071428571428571175, 0.5142857142857142350, 0.5214285714285714635, 0.5285714285714285809, 0.5357142857142856984, 0.5428571428571428159, 0.5500000000000000444, 0.5571428571428571619, 0.5642857142857142794, 0.5714285714285713969, 0.5785714285714286254, 0.5857142857142857428, 0.5928571428571428603, 0.5999999999999999778, 0.6071428571428570953, 0.6142857142857143238, 0.6214285714285714413, 0.6285714285714285587, 0.6357142857142856762, 0.6428571428571429047, 0.6500000000000000222, 0.6571428571428571397, 0.6642857142857142572, 0.6714285714285713746, 0.6785714285714286031, 0.6857142857142857206, 0.6928571428571428381, 0.6999999999999999556, 0.7071428571428571841, 0.7142857142857143016, 0.7214285714285714191, 0.7285714285714285365, 0.7357142857142857650, 0.7428571428571428825, 0.7500000000000000000, 0.7571428571428571175, 0.7642857142857142350, 0.7714285714285714635, 0.7785714285714285809, 0.7857142857142856984, 0.7928571428571428159, 0.8000000000000000444, 0.8071428571428571619, 0.8142857142857142794, 0.8214285714285713969, 0.8285714285714286254, 0.8357142857142857428, 0.8428571428571428603, 0.8499999999999999778, 0.8571428571428570953, 0.8642857142857143238, 0.8714285714285714413, 0.8785714285714285587, 0.8857142857142856762, 0.8928571428571429047, 0.9000000000000000222, 0.9071428571428571397, 0.9142857142857142572, 0.9214285714285713746, 0.9285714285714286031, 0.9357142857142857206, 0.9428571428571428381, 0.9499999999999999556, 0.9523897249335834259 ),
 .UNSPECIFIED. ) 
 GEOMETRIC_REPRESENTATION_ITEM ( )  RATIONAL_B_SPLINE_SURFACE ( (
 ( 1.000000000000000000, 0.9510565162951535312, 1.000000000000000000, 0.9510565162951535312, 1.000000000000000000, 0.9510565162951535312, 1.000000000000000000, 0.9510565162951535312, 1.000000000000000000, 0.9510565162951535312, 1.000000000000000000, 0.9510565162951535312, 1.000000000000000000, 0.9510565162951535312, 1.000000000000000000, 0.9510565162951535312, 1.000000000000000000, 0.9510565162951535312, 1.000000000000000000, 0.9510565162951535312, 1.000000000000000000, 0.9510565162951535312, 1.000000000000000000, 0.9510565162951535312, 1.000000000000000000, 0.9510565162951535312, 1.000000000000000000, 0.9510565162951535312, 1.000000000000000000, 0.9510565162951535312, 1.000000000000000000, 0.9510565162951535312, 1.000000000000000000, 0.9510565162951535312, 1.000000000000000000, 0.9510565162951535312, 1.000000000000000000, 0.9510565162951535312, 1.000000000000000000, 0.9510565162951535312, 1.000000000000000000, 0.9510565162951535312, 1.000000000000000000, 0.9510565162951535312, 1.000000000000000000, 0.9510565162951535312, 1.000000000000000000, 0.9510565162951535312, 1.000000000000000000, 0.9510565162951535312, 1.000000000000000000, 0.9510565162951535312, 1.000000000000000000, 0.9510565162951535312, 1.000000000000000000, 0.9510565162951535312, 1.000000000000000000, 0.9510565162951535312, 1.000000000000000000, 0.9510565162951535312, 1.000000000000000000, 0.9510565162951535312, 1.000000000000000000, 0.9510565162951535312, 1.000000000000000000, 0.9510565162951535312, 1.000000000000000000, 0.9510565162951535312, 1.000000000000000000, 0.9510565162951535312, 1.000000000000000000, 0.9510565162951535312, 1.000000000000000000, 0.9510565162951535312, 1.000000000000000000, 0.9510565162951535312, 1.000000000000000000, 0.9510565162951535312, 1.000000000000000000, 0.9510565162951535312, 1.000000000000000000, 0.9510565162951535312, 1.000000000000000000, 0.9510565162951535312, 1.000000000000000000, 0.9510565162951535312, 1.000000000000000000, 0.9510565162951535312, 1.000000000000000000, 0.9510565162951535312, 1.000000000000000000, 0.9510565162951535312, 1.000000000000000000, 0.9510565162951535312, 1.000000000000000000, 0.9510565162951535312, 1.000000000000000000, 0.9510565162951535312, 1.000000000000000000, 0.9510565162951535312, 1.000000000000000000, 0.9510565162951535312, 1.000000000000000000, 0.9510565162951535312, 1.000000000000000000, 0.9510565162951535312, 1.000000000000000000, 0.9510565162951535312, 1.000000000000000000, 0.9510565162951535312, 1.000000000000000000, 0.9510565162951535312, 1.000000000000000000, 0.9510565162951535312, 1.000000000000000000, 0.9510565162951535312, 1.000000000000000000, 0.9510565162951535312, 1.000000000000000000, 0.9510565162951535312, 1.000000000000000000, 0.9510565162951535312, 1.000000000000000000, 0.9510565162951535312, 1.000000000000000000, 0.9510565162951535312, 1.000000000000000000, 0.9510565162951535312, 1.000000000000000000, 0.9510565162951535312, 1.000000000000000000, 0.9510565162951535312, 1.000000000000000000, 0.9510565162951535312, 1.000000000000000000, 0.9510565162951535312, 1.000000000000000000, 0.9510565162951535312, 1.000000000000000000, 0.9510565162951535312, 1.000000000000000000, 0.9510565162951535312, 1.000000000000000000, 0.9510565162951535312, 1.000000000000000000, 0.9510565162951535312, 1.000000000000000000, 0.9510565162951535312, 1.000000000000000000, 0.9510565162951535312, 1.000000000000000000, 0.9510565162951535312, 1.000000000000000000, 0.9510565162951535312, 1.000000000000000000, 0.9510565162951535312, 1.000000000000000000, 0.9510565162951535312, 1.000000000000000000, 0.9510565162951535312, 1.000000000000000000, 0.9510565162951535312, 1.000000000000000000, 0.9510565162951535312, 1.000000000000000000, 0.9510565162951535312, 1.000000000000000000, 0.9510565162951535312, 1.000000000000000000, 0.9510565162951535312, 1.000000000000000000, 0.9510565162951535312, 1.000000000000000000, 0.9510565162951535312, 1.000000000000000000, 0.9510565162951535312, 1.000000000000000000, 0.9510565162951535312, 1.000000000000000000, 0.9510565162951535312, 1.000000000000000000, 0.9510565162951535312, 1.000000000000000000, 0.9510565162951535312, 1.000000000000000000, 0.9510565162951535312, 1.000000000000000000, 0.9510565162951535312, 1.000000000000000000, 0.9510565162951535312, 1.000000000000000000, 0.9510565162951535312, 1.000000000000000000, 0.9510565162951535312, 1.000000000000000000, 0.9510565162951535312, 1.000000000000000000, 0.9510565162951535312, 1.000000000000000000, 0.9510565162951535312, 1.000000000000000000, 0.9510565162951535312, 1.000000000000000000, 0.9510565162951535312, 1.000000000000000000, 0.9510565162951535312, 1.000000000000000000, 0.9510565162951535312, 1.000000000000000000, 0.9510565162951535312, 1.000000000000000000, 0.9510565162951535312, 1.000000000000000000, 0.9510565162951535312, 1.000000000000000000, 0.9510565162951535312, 1.000000000000000000, 0.9510565162951535312, 1.000000000000000000, 0.9510565162951535312, 1.000000000000000000, 0.9510565162951535312, 1.000000000000000000, 0.9510565162951535312, 1.000000000000000000, 0.9510565162951535312, 1.000000000000000000, 0.9510565162951535312, 1.000000000000000000, 0.9510565162951535312, 1.000000000000000000, 0.9510565162951535312, 1.000000000000000000, 0.9510565162951535312, 1.000000000000000000, 0.9510565162951535312, 1.000000000000000000, 0.9510565162951535312, 1.000000000000000000, 0.9510565162951535312, 1.000000000000000000, 0.9510565162951535312, 1.000000000000000000, 0.9510565162951535312, 1.000000000000000000, 0.9510565162951535312, 1.000000000000000000, 0.9510565162951535312, 1.000000000000000000, 0.9510565162951535312, 1.000000000000000000, 0.9510565162951535312, 1.000000000000000000, 0.9510565162951535312, 1.000000000000000000, 0.9510565162951535312, 1.000000000000000000, 0.9510565162951535312, 1.000000000000000000, 0.9510565162951535312, 1.000000000000000000, 0.9510565162951535312, 1.000000000000000000, 0.9510565162951535312, 1.000000000000000000, 0.9510565162951535312, 1.000000000000000000, 0.9836253951315730992, 0.9782074146920101132),
 ( 1.000000000000000000, 0.9510565162951535312, 1.000000000000000000, 0.9510565162951535312, 1.000000000000000000, 0.9510565162951535312, 1.000000000000000000, 0.9510565162951535312, 1.000000000000000000, 0.9510565162951535312, 1.000000000000000000, 0.9510565162951535312, 1.000000000000000000, 0.9510565162951535312, 1.000000000000000000, 0.9510565162951535312, 1.000000000000000000, 0.9510565162951535312, 1.000000000000000000, 0.9510565162951535312, 1.000000000000000000, 0.9510565162951535312, 1.000000000000000000, 0.9510565162951535312, 1.000000000000000000, 0.9510565162951535312, 1.000000000000000000, 0.9510565162951535312, 1.000000000000000000, 0.9510565162951535312, 1.000000000000000000, 0.9510565162951535312, 1.000000000000000000, 0.9510565162951535312, 1.000000000000000000, 0.9510565162951535312, 1.000000000000000000, 0.9510565162951535312, 1.000000000000000000, 0.9510565162951535312, 1.000000000000000000, 0.9510565162951535312, 1.000000000000000000, 0.9510565162951535312, 1.000000000000000000, 0.9510565162951535312, 1.000000000000000000, 0.9510565162951535312, 1.000000000000000000, 0.9510565162951535312, 1.000000000000000000, 0.9510565162951535312, 1.000000000000000000, 0.9510565162951535312, 1.000000000000000000, 0.9510565162951535312, 1.000000000000000000, 0.9510565162951535312, 1.000000000000000000, 0.9510565162951535312, 1.000000000000000000, 0.9510565162951535312, 1.000000000000000000, 0.9510565162951535312, 1.000000000000000000, 0.9510565162951535312, 1.000000000000000000, 0.9510565162951535312, 1.000000000000000000, 0.9510565162951535312, 1.000000000000000000, 0.9510565162951535312, 1.000000000000000000, 0.9510565162951535312, 1.000000000000000000, 0.9510565162951535312, 1.000000000000000000, 0.9510565162951535312, 1.000000000000000000, 0.9510565162951535312, 1.000000000000000000, 0.9510565162951535312, 1.000000000000000000, 0.9510565162951535312, 1.000000000000000000, 0.9510565162951535312, 1.000000000000000000, 0.9510565162951535312, 1.000000000000000000, 0.9510565162951535312, 1.000000000000000000, 0.9510565162951535312, 1.000000000000000000, 0.9510565162951535312, 1.000000000000000000, 0.9510565162951535312, 1.000000000000000000, 0.9510565162951535312, 1.000000000000000000, 0.9510565162951535312, 1.000000000000000000, 0.9510565162951535312, 1.000000000000000000, 0.9510565162951535312, 1.000000000000000000, 0.9510565162951535312, 1.000000000000000000, 0.9510565162951535312, 1.000000000000000000, 0.9510565162951535312, 1.000000000000000000, 0.9510565162951535312, 1.000000000000000000, 0.9510565162951535312, 1.000000000000000000, 0.9510565162951535312, 1.000000000000000000, 0.9510565162951535312, 1.000000000000000000, 0.9510565162951535312, 1.000000000000000000, 0.9510565162951535312, 1.000000000000000000, 0.9510565162951535312, 1.000000000000000000, 0.9510565162951535312, 1.000000000000000000, 0.9510565162951535312, 1.000000000000000000, 0.9510565162951535312, 1.000000000000000000, 0.9510565162951535312, 1.000000000000000000, 0.9510565162951535312, 1.000000000000000000, 0.9510565162951535312, 1.000000000000000000, 0.9510565162951535312, 1.000000000000000000, 0.9510565162951535312, 1.000000000000000000, 0.9510565162951535312, 1.000000000000000000, 0.9510565162951535312, 1.000000000000000000, 0.9510565162951535312, 1.000000000000000000, 0.9510565162951535312, 1.000000000000000000, 0.9510565162951535312, 1.000000000000000000, 0.9510565162951535312, 1.000000000000000000, 0.9510565162951535312, 1.000000000000000000, 0.9510565162951535312, 1.000000000000000000, 0.9510565162951535312, 1.000000000000000000, 0.9510565162951535312, 1.000000000000000000, 0.9510565162951535312, 1.000000000000000000, 0.9510565162951535312, 1.000000000000000000, 0.9510565162951535312, 1.000000000000000000, 0.9510565162951535312, 1.000000000000000000, 0.9510565162951535312, 1.000000000000000000, 0.9510565162951535312, 1.000000000000000000, 0.9510565162951535312, 1.000000000000000000, 0.9510565162951535312, 1.000000000000000000, 0.9510565162951535312, 1.000000000000000000, 0.9510565162951535312, 1.000000000000000000, 0.9510565162951535312, 1.000000000000000000, 0.9510565162951535312, 1.000000000000000000, 0.9510565162951535312, 1.000000000000000000, 0.9510565162951535312, 1.000000000000000000, 0.9510565162951535312, 1.000000000000000000, 0.9510565162951535312, 1.000000000000000000, 0.9510565162951535312, 1.000000000000000000, 0.9510565162951535312, 1.000000000000000000, 0.9510565162951535312, 1.000000000000000000, 0.9510565162951535312, 1.000000000000000000, 0.9510565162951535312, 1.000000000000000000, 0.9510565162951535312, 1.000000000000000000, 0.9510565162951535312, 1.000000000000000000, 0.9510565162951535312, 1.000000000000000000, 0.9510565162951535312, 1.000000000000000000, 0.9510565162951535312, 1.000000000000000000, 0.9510565162951535312, 1.000000000000000000, 0.9510565162951535312, 1.000000000000000000, 0.9510565162951535312, 1.000000000000000000, 0.9510565162951535312, 1.000000000000000000, 0.9510565162951535312, 1.000000000000000000, 0.9510565162951535312, 1.000000000000000000, 0.9510565162951535312, 1.000000000000000000, 0.9510565162951535312, 1.000000000000000000, 0.9510565162951535312, 1.000000000000000000, 0.9510565162951535312, 1.000000000000000000, 0.9510565162951535312, 1.000000000000000000, 0.9510565162951535312, 1.000000000000000000, 0.9510565162951535312, 1.000000000000000000, 0.9510565162951535312, 1.000000000000000000, 0.9510565162951535312, 1.000000000000000000, 0.9510565162951535312, 1.000000000000000000, 0.9510565162951535312, 1.000000000000000000, 0.9510565162951535312, 1.000000000000000000, 0.9510565162951535312, 1.000000000000000000, 0.9510565162951535312, 1.000000000000000000, 0.9510565162951535312, 1.000000000000000000, 0.9510565162951535312, 1.000000000000000000, 0.9510565162951535312, 1.000000000000000000, 0.9510565162951535312, 1.000000000000000000, 0.9510565162951535312, 1.000000000000000000, 0.9510565162951535312, 1.000000000000000000, 0.9510565162951535312, 1.000000000000000000, 0.9836253951315730992, 0.9782074146920101132) ) ) 
 REPRESENTATION_ITEM ( '' )  SURFACE ( )  );
#768 = CARTESIAN_POINT ( 'NONE',  ( 44.55648932407425633, 90.68445800887258201, 38.96596240072933170 ) ) ;
#769 = CARTESIAN_POINT ( 'NONE',  ( 47.43856463449118621, 148.8797705074273097, 34.21067981925357060 ) ) ;
#770 = AXIS2_PLACEMENT_3D ( 'NONE', #10420, #3801, #12272 ) ;
#771 = AXIS2_PLACEMENT_3D ( 'NONE', #11380, #1580, #9853 ) ;
#772 = CARTESIAN_POINT ( 'NONE',  ( 38.96631938032478359, 145.0104996726487627, 37.14960608071593384 ) ) ;
#774 = CARTESIAN_POINT ( 'NONE',  ( 32.71008791447857789, 146.0719641954536883, -2.505641559509553140 ) ) ;
#773 = CARTESIAN_POINT ( 'NONE',  ( 40.27526882409969033, 102.5651871740939782, 37.97664729208901946 ) ) ;
#775 = CARTESIAN_POINT ( 'NONE',  ( 44.55648932407425633, 59.81049967264874567, 29.45539723777780239 ) ) ;
#777 = CARTESIAN_POINT ( 'NONE',  ( -143.3790856849358306, -183.3630981290893374, 55.53486410454105027 ) ) ;
#776 = CARTESIAN_POINT ( 'NONE',  ( 45.52055293674428071, 144.7823678009017954, 38.54804764342389944 ) ) ;
#778 = CARTESIAN_POINT ( 'NONE',  ( -151.4692556286852891, -186.8130981290893260, 59.65701158161632378 ) ) ;
#779 = DIRECTION ( 'NONE',  ( 0.000000000000000000, 0.000000000000000000, 1.000000000000000000 ) ) ;
#780 = CARTESIAN_POINT ( 'NONE',  ( 39.42975644700377558, 66.41518717409400097, 36.81289934271958941 ) ) ;
#781 = DIRECTION ( 'NONE',  ( 0.9387810623359076345, 0.3426822732243071656, 0.03548206049944094970 ) ) ;
#782 = CARTESIAN_POINT ( 'NONE',  ( -154.3824083646099439, -173.4938272943107336, 40.69124936498395328 ) ) ;
#783 = CARTESIAN_POINT ( 'NONE',  ( -145.6429501568359797, -195.2084106276440423, 41.63779006702063867 ) ) ;
#784 = VERTEX_POINT ( 'NONE', #6929 ) ;
#785 = CARTESIAN_POINT ( 'NONE',  ( 51.15470623622070434, 86.57325545146775880, 6.072769092256255163 ) ) ;
#786 = CARTESIAN_POINT ( 'NONE',  ( -130.4480969619998234, -126.9891397928655010, 67.64809332337415526 ) ) ;
#787 = AXIS2_PLACEMENT_3D ( 'NONE', #2416, #20942, #338 ) ;
#788 = CARTESIAN_POINT ( 'NONE',  ( 38.58424406990784661, 146.9651871740940123, 32.77220824515698183 ) ) ;
#789 = CARTESIAN_POINT ( 'NONE',  ( 43.01140435219951286, 155.3651871740940180, 29.55568802177586107 ) ) ;
#790 = CARTESIAN_POINT ( 'NONE',  ( 38.58424406990785371, 105.5297705074273011, 35.64915139335015937 ) ) ;
#791 = ORIENTED_EDGE ( 'NONE', *, *, #18308, .F. ) ;
#792 = EDGE_LOOP ( 'NONE', ( #7745, #13828, #225, #21173 ) ) ;
#793 = CARTESIAN_POINT ( 'NONE',  ( 67.98812442775457043, 106.8157236907426153, -0.7957547315468347371 ) ) ;
#794 = ORIENTED_EDGE ( 'NONE', *, *, #18272, .F. ) ;
#795 = CARTESIAN_POINT ( 'NONE',  ( 44.55648932407425633, 114.6844580088725820, 38.96596240072933170 ) ) ;
#796 = CARTESIAN_POINT ( 'NONE',  ( 47.05648932407426344, 89.51049967264873430, 31.27175355779120025 ) ) ;
#797 = CARTESIAN_POINT ( 'NONE',  ( 39.42975644700377558, 78.67977050742732104, 36.81289934271958941 ) ) ;
#798 = CARTESIAN_POINT ( 'NONE',  ( 47.43856463449117200, 133.4651871740940123, 35.64915139335016647 ) ) ;
#799 = CARTESIAN_POINT ( 'NONE',  ( 38.96631938032478359, 102.4104996726487400, 31.27175355779120025 ) ) ;
#800 = CARTESIAN_POINT ( 'NONE',  ( 75.16956835342354282, 131.6452004531123805, 5.196376467030073165 ) ) ;
#801 = CARTESIAN_POINT ( 'NONE',  ( 47.05648932407426344, 119.5104996726487343, 31.27175355779120025 ) ) ;
#802 = CARTESIAN_POINT ( 'NONE',  ( -148.3790856849358306, -162.3891397928654499, 40.14644641866477315 ) ) ;
#803 = DIRECTION ( 'NONE',  ( 0.000000000000000000, 0.000000000000000000, 1.000000000000000000 ) ) ;
#804 = CYLINDRICAL_SURFACE ( 'NONE', #5889, 10.00000000000000888 ) ;
#805 = LINE ( 'NONE', #10631, #5353 ) ;
#806 = ORIENTED_EDGE ( 'NONE', *, *, #5935, .F. ) ;
#807 = CARTESIAN_POINT ( 'NONE',  ( 45.74753988029933538, 88.42977050742729261, 37.97664729208901946 ) ) ;
#808 = CARTESIAN_POINT ( 'NONE',  ( -148.5561028927606344, -162.9938272943107336, 58.62277379824867296 ) ) ;
#809 = CARTESIAN_POINT ( 'NONE',  ( 75.85495621331871519, 129.5603373922052697, -8.732165470513974626 ) ) ;
#810 = CARTESIAN_POINT ( 'NONE',  ( -160.8964159109769696, -191.0084106276440821, 52.72008163687743121 ) ) ;
#811 = VERTEX_POINT ( 'NONE', #13743 ) ;
#812 = CARTESIAN_POINT ( 'NONE',  ( -154.5594255724347761, -174.9630981290893033, 59.16757674456785310 ) ) ;
#813 = CYLINDRICAL_SURFACE ( 'NONE', #17657, 4.999999999999997335 ) ;
#814 = CARTESIAN_POINT ( 'NONE',  ( 38.58424406990785371, 135.2297705074273324, 32.77220824515697473 ) ) ;
#815 = CARTESIAN_POINT ( 'NONE',  ( 15.58850788081759475, 140.2644050767460442, -10.20415289822252980 ) ) ;
#816 = ORIENTED_EDGE ( 'NONE', *, *, #1747, .T. ) ;
#817 = CARTESIAN_POINT ( 'NONE',  ( 43.80332655382220253, 72.61133943119284595, 39.21067981925355639 ) ) ;
#818 = ORIENTED_EDGE ( 'NONE', *, *, #4976, .F. ) ;
#819 = CARTESIAN_POINT ( 'NONE',  ( 39.42975644700377558, 126.0797705074273267, 31.60846029578754468 ) ) ;
#820 = CARTESIAN_POINT ( 'NONE',  ( 46.10157429594899270, 144.8344580088725877, 38.46393386101375711 ) ) ;
#821 = CARTESIAN_POINT ( 'NONE',  ( 40.27526882409969033, 93.82977050742731251, 37.97664729208901946 ) ) ;
#822 = CARTESIAN_POINT ( 'NONE',  ( 43.01140435219951996, 154.4604996726487798, 39.21067981925357060 ) ) ;
#823 = CARTESIAN_POINT ( 'NONE',  ( 43.01140435219951286, 100.4604996726487371, 39.21067981925356349 ) ) ;
#824 = CARTESIAN_POINT ( 'NONE',  ( 39.92123440845005433, 129.2604996726487343, 29.95742577749336988 ) ) ;
#825 = CARTESIAN_POINT ( 'NONE',  ( -145.2889157411863437, -191.6130981290893089, 41.15050349809589392 ) ) ;
#826 = CARTESIAN_POINT ( 'NONE',  ( -160.8964159109769696, -158.0084106276440536, 52.72008163687743121 ) ) ;
#827 = EDGE_CURVE ( 'NONE', #3465, #5698, #13959, .T. ) ;
#828 =( BOUNDED_CURVE ( )  B_SPLINE_CURVE ( 2, ( #10493, #14000, #5408, #2107, #20734, #15765, #8844, #5735, #669, #17411, #12126, #17303, #2317 ),
 .UNSPECIFIED., .F., .F. ) 
 B_SPLINE_CURVE_WITH_KNOTS ( ( 3, 2, 2, 2, 2, 2, 3 ),
 ( 0.5178571428571429047, 0.5214285714285714635, 0.5285714285714285809, 0.5357142857142856984, 0.5428571428571428159, 0.5500000000000000444, 0.5535714285714286031 ),
 .UNSPECIFIED. ) 
 CURVE ( )  GEOMETRIC_REPRESENTATION_ITEM ( )  RATIONAL_B_SPLINE_CURVE ( ( 0.9755282581475768211, 0.9755282581475771542, 1.000000000000000000, 0.9510565162951535312, 1.000000000000000000, 0.9510565162951535312, 1.000000000000000000, 0.9510565162951535312, 1.000000000000000000, 0.9510565162951535312, 1.000000000000000000, 0.9755282581475768211, 0.9755282581475768211 ) ) 
 REPRESENTATION_ITEM ( '' )  );
#829 = CARTESIAN_POINT ( 'NONE',  ( 47.43856463449117200, 97.76518717409398107, 32.77220824515698183 ) ) ;
#830 = CARTESIAN_POINT ( 'NONE',  ( 48.01140435219951996, 74.21049967264873715, 34.21067981925357060 ) ) ;
#831 = DIRECTION ( 'NONE',  ( -0.000000000000000000, 1.000000000000000000, -0.000000000000000000 ) ) ;
#832 = CARTESIAN_POINT ( 'NONE',  ( -161.4692556286853176, -157.5630981290892976, 49.65701158161630957 ) ) ;
#833 = CARTESIAN_POINT ( 'NONE',  ( 39.92123440845005433, 132.2344580088725650, 38.46393386101375711 ) ) ;
#834 = CARTESIAN_POINT ( 'NONE',  ( 48.01140435219951996, 130.1344580088725422, 35.83527830041810347 ) ) ;
#835 = CARTESIAN_POINT ( 'NONE',  ( 44.37947211624943833, 115.2797705074273296, 38.42115945441014446 ) ) ;
#836 = CARTESIAN_POINT ( 'NONE',  ( 29.49905557571407044, 144.7517438296894738, 9.366394860000250233 ) ) ;
#837 = CARTESIAN_POINT ( 'NONE',  ( -159.0959885057557983, -190.5938272943107279, 55.19815736654470584 ) ) ;
#838 = CARTESIAN_POINT ( 'NONE',  ( 41.64333658814960870, 93.71518717409401233, 38.42115945441014446 ) ) ;
#839 = CARTESIAN_POINT ( 'NONE',  ( 38.96631938032478359, 91.01049967264873430, 37.14960608071593384 ) ) ;
#840 = ORIENTED_EDGE ( 'NONE', *, *, #12750, .F. ) ;
#841 = DIRECTION ( 'NONE',  ( 0.000000000000000000, 1.000000000000000000, 0.000000000000000000 ) ) ;
#842 = CARTESIAN_POINT ( 'NONE',  ( 18.20936163119166196, 143.5026679720446907, 2.934308097026923967 ) ) ;
#843 = CARTESIAN_POINT ( 'NONE',  ( 65.44800906011916197, 136.9904114405718758, 11.94221925691594777 ) ) ;
#844 = CARTESIAN_POINT ( 'NONE',  ( 20.98687704487253569, 141.7792436784441747, -11.00219731500033049 ) ) ;
#845 = CARTESIAN_POINT ( 'NONE',  ( 46.59305225739526435, 76.57977050742731251, 36.81289934271958941 ) ) ;
#846 = VERTEX_POINT ( 'NONE', #3620 ) ;
#847 = ORIENTED_EDGE ( 'NONE', *, *, #6809, .F. ) ;
#848 = CARTESIAN_POINT ( 'NONE',  ( 38.58424406990786082, 159.3797705074273381, 34.21067981925357060 ) ) ;
#849 = LINE ( 'NONE', #21030, #3140 ) ;
#850 = AXIS2_PLACEMENT_3D ( 'NONE', #17976, #8078, #1233 ) ;
#851 = CARTESIAN_POINT ( 'NONE',  ( 38.96631938032478359, 120.4104996726487400, 31.27175355779120025 ) ) ;
#853 = CARTESIAN_POINT ( 'NONE',  ( 9.783399875253829592, 127.8057224500684015, -3.656374068424393275 ) ) ;
#852 = CARTESIAN_POINT ( 'NONE',  ( 39.42975644700377558, 80.81518717409400665, 31.60846029578754468 ) ) ;
#854 = CARTESIAN_POINT ( 'NONE',  ( -160.8964159109769696, -167.0438272943106881, 46.59394152635518083 ) ) ;
#855 = CARTESIAN_POINT ( 'NONE',  ( 70.26356658872128946, 140.6255928306487704, 11.86290872716119615 ) ) ;
#856 = CARTESIAN_POINT ( 'NONE',  ( -151.4692556286852891, -183.8130981290892692, 60.17163382399899518 ) ) ;
#857 =( LENGTH_UNIT ( ) NAMED_UNIT ( * ) SI_UNIT ( .MILLI., .METRE. ) );
#858 = DIRECTION ( 'NONE',  ( 1.000000000000000000, 0.000000000000000000, 5.966140889015784385E-16 ) ) ;
#859 = CARTESIAN_POINT ( 'NONE',  ( 47.05648932407426344, 156.9844580088725934, 37.14960608071593384 ) ) ;
#860 = CARTESIAN_POINT ( 'NONE',  ( 44.37947211624943833, 140.4797705074273324, 30.00020018409699318 ) ) ;
#861 = CARTESIAN_POINT ( 'NONE',  ( 10.61292492956169475, 108.6005711365770026, 0.7156557588857267449 ) ) ;
#862 = CARTESIAN_POINT ( 'NONE',  ( 41.64333658814960870, 123.7151871740940123, 38.42115945441014446 ) ) ;
#863 =( NAMED_UNIT ( * ) SI_UNIT ( $, .STERADIAN. ) SOLID_ANGLE_UNIT ( ) );
#864 = CARTESIAN_POINT ( 'NONE',  ( -145.6429501568359797, -156.2084106276440423, 41.63779006702063867 ) ) ;
#865 = EDGE_CURVE ( 'NONE', #890, #8983, #9337, .T. ) ;
#866 = CARTESIAN_POINT ( 'NONE',  ( -159.5594255724347761, -164.1891397928654897, 55.53486410454104316 ) ) ;
#867 = CYLINDRICAL_SURFACE ( 'NONE', #16262, 88.09373137032866907 ) ;
#868 = EDGE_CURVE ( 'NONE', #19655, #14419, #11582, .T. ) ;
#869 = CARTESIAN_POINT ( 'NONE',  ( 43.17520790721623314, 91.62706341066298421, 13.41396976009479403 ) ) ;
#870 = CARTESIAN_POINT ( 'NONE',  ( 42.21948215057684450, 121.3836182503284533, 39.21067981925355639 ) ) ;
#871 = CARTESIAN_POINT ( 'NONE',  ( 39.42975644700377558, 104.8151871740939924, 31.60846029578754468 ) ) ;
#872 = VERTEX_POINT ( 'NONE', #20055 ) ;
#873 = CARTESIAN_POINT ( 'NONE',  ( 44.55648932407425633, 85.61049967264872862, 38.96596240072933170 ) ) ;
#874 = ORIENTED_EDGE ( 'NONE', *, *, #1015, .F. ) ;
#875 = CARTESIAN_POINT ( 'NONE',  ( 39.92123440845004723, 96.23445800887257917, 38.46393386101376421 ) ) ;
#876 = CARTESIAN_POINT ( 'NONE',  ( 43.01140435219951286, 146.9604996726486945, 28.95336869806222779 ) ) ;
#878 = CARTESIAN_POINT ( 'NONE',  ( 14.99696000743431235, 117.4761687382565327, -3.934212988072375516 ) ) ;
#877 = CARTESIAN_POINT ( 'NONE',  ( 47.43856463449117200, 106.7651871740939811, 32.77220824515698183 ) ) ;
#879 = LINE ( 'NONE', #9488, #12922 ) ;
#881 = CARTESIAN_POINT ( 'NONE',  ( -151.4692556286852607, -156.8130981290892692, 59.65701158161632378 ) ) ;
#880 = CARTESIAN_POINT ( 'NONE',  ( -154.5594255724347761, -167.1630981290892919, 40.14644641866476604 ) ) ;
#882 = EDGE_CURVE ( 'NONE', #1447, #4126, #15074, .T. ) ;
#883 = FACE_OUTER_BOUND ( 'NONE', #16754, .T. ) ;
#884 = LINE ( 'NONE', #9271, #9392 ) ;
#885 = CARTESIAN_POINT ( 'NONE',  ( 38.58424406990784661, 71.96518717409399812, 32.77220824515698183 ) ) ;
#886 = DIRECTION ( 'NONE',  ( -1.000000000000000000, 0.000000000000000000, 0.000000000000000000 ) ) ;
#887 = CARTESIAN_POINT ( 'NONE',  ( 38.01140435219952707, 114.7104996726487371, 34.21067981925357060 ) ) ;
#888 = CARTESIAN_POINT ( 'NONE',  ( -151.4692556286852891, -167.6438272943107108, 39.74470866294723947 ) ) ;
#889 = DIRECTION ( 'NONE',  ( 1.000000000000000000, -0.000000000000000000, -0.000000000000000000 ) ) ;
#890 = VERTEX_POINT ( 'NONE', #11652 ) ;
#891 = CARTESIAN_POINT ( 'NONE',  ( 54.37136329154349568, 152.2862128563062072, 3.215626235130811583 ) ) ;
#892 = EDGE_LOOP ( 'NONE', ( #21201, #9511, #8668, #6236 ) ) ;
#893 = CARTESIAN_POINT ( 'NONE',  ( 38.58424406990784661, 132.2651871740939953, 35.64915139335016647 ) ) ;
#894 =( BOUNDED_CURVE ( )  B_SPLINE_CURVE ( 2, ( #2570, #4122, #20991, #5548, #8879, #5768, #10532, #13928, #13824, #12275, #5447, #12497, #15586 ),
 .UNSPECIFIED., .F., .F. ) 
 B_SPLINE_CURVE_WITH_KNOTS ( ( 3, 2, 2, 2, 2, 2, 3 ),
 ( 0.7132352941176470784, 0.7147058823529411908, 0.7176470588235294157, 0.7205882352941176405, 0.7235294117647058654, 0.7264705882352940902, 0.7279411764705882026 ),
 .UNSPECIFIED. ) 
 CURVE ( )  GEOMETRIC_REPRESENTATION_ITEM ( )  RATIONAL_B_SPLINE_CURVE ( ( 0.9755282581475768211, 0.9755282581475768211, 1.000000000000000000, 0.9510565162951535312, 1.000000000000000000, 0.9510565162951535312, 1.000000000000000000, 0.9510565162951535312, 1.000000000000000000, 0.9510565162951535312, 1.000000000000000000, 0.9755282581475768211, 0.9755282581475768211 ) ) 
 REPRESENTATION_ITEM ( '' )  );
#895 = CARTESIAN_POINT ( 'NONE',  ( 41.64333658814960870, 95.77977050742732956, 30.00020018409699318 ) ) ;
#896 = ORIENTED_EDGE ( 'NONE', *, *, #16906, .F. ) ;
#897 = ORIENTED_EDGE ( 'NONE', *, *, #12786, .F. ) ;
#898 = CARTESIAN_POINT ( 'NONE',  ( 39.35338560254503903, 91.94623120232463975, 14.56122079753911081 ) ) ;
#899 = ORIENTED_EDGE ( 'NONE', *, *, #19930, .T. ) ;
#900 = VECTOR ( 'NONE', #10656, 1000.000000000000114 ) ;
#901 = CARTESIAN_POINT ( 'NONE',  ( 44.37947211624943833, 79.27977050742731535, 38.42115945441014446 ) ) ;
#902 = CARTESIAN_POINT ( 'NONE',  ( 39.42975644700377558, 131.8151871740940067, 31.60846029578754468 ) ) ;
#903 = CARTESIAN_POINT ( 'NONE',  ( 48.01140435219951996, 92.06049967264871725, 35.83527830041810347 ) ) ;
#904 = CARTESIAN_POINT ( 'NONE',  ( 62.84376099716368458, 92.00366499689042143, 13.64888190966157566 ) ) ;
#905 = EDGE_CURVE ( 'NONE', #6804, #17969, #16936, .T. ) ;
#906 = CARTESIAN_POINT ( 'NONE',  ( 138.2149183826930425, 102.3264679885537305, 14.00000000000001776 ) ) ;
#907 = CARTESIAN_POINT ( 'NONE',  ( -141.4692556286852891, -159.9891397928654726, 49.65701158161630957 ) ) ;
#908 = CARTESIAN_POINT ( 'NONE',  ( -148.3790856849358306, -159.6630981290892919, 59.16757674456786020 ) ) ;
#909 = CARTESIAN_POINT ( 'NONE',  ( -27.64582385433944367, -84.13255853780189852, 5.000000000000018652 ) ) ;
#910 = CARTESIAN_POINT ( 'NONE',  ( 44.55648932407425633, 106.8844580088725849, 29.45539723777780239 ) ) ;
#911 = CIRCLE ( 'NONE', #16036, 88.09373137032866907 ) ;
#912 = EDGE_LOOP ( 'NONE', ( #15164, #18877, #13960, #16804 ) ) ;
#913 = CARTESIAN_POINT ( 'NONE',  ( 47.43856463449117200, 71.02977050742730114, 32.77220824515698183 ) ) ;
#914 = CARTESIAN_POINT ( 'NONE',  ( -154.3824083646099439, -169.2938272943107165, 58.62277379824867296 ) ) ;
#915 = CARTESIAN_POINT ( 'NONE',  ( 15.75986397150585816, 99.18880659646561071, -5.637120474378671808 ) ) ;
#916 = CARTESIAN_POINT ( 'NONE',  ( -157.2955611005346270, -194.6084106276440195, 41.63779006702063867 ) ) ;
#917 = CIRCLE ( 'NONE', #14285, 21.90454335994854063 ) ;
#918 = ORIENTED_EDGE ( 'NONE', *, *, #19173, .F. ) ;
#919 = CARTESIAN_POINT ( 'NONE',  ( 5.130598475945862827E-15, 0.000000000000000000, 20.00000000000001776 ) ) ;
#920 = CIRCLE ( 'NONE', #13247, 10.00000000000000888 ) ;
#921 = CARTESIAN_POINT ( 'NONE',  ( 38.01140435219952707, 104.9344580088725820, 35.83527830041809636 ) ) ;
#922 = CARTESIAN_POINT ( 'NONE',  ( 41.64333658814960870, 120.9797705074273182, 38.42115945441014446 ) ) ;
#923 = ORIENTED_EDGE ( 'NONE', *, *, #17652, .T. ) ;
#924 = CARTESIAN_POINT ( 'NONE',  ( 43.80332655382220253, 73.95757658655232092, 29.21067981925356705 ) ) ;
#925 = ORIENTED_EDGE ( 'NONE', *, *, #19064, .F. ) ;
#926 = CARTESIAN_POINT ( 'NONE',  ( 46.59305225739526435, 131.1797705074273210, 31.60846029578754468 ) ) ;
#927 = CARTESIAN_POINT ( 'NONE',  ( 43.01140435219951286, 134.9604996726487514, 29.21067981925356705 ) ) ;
#928 = AXIS2_PLACEMENT_3D ( 'NONE', #10600, #15343, #18757 ) ;
#929 = EDGE_CURVE ( 'NONE', #15878, #9201, #3287, .T. ) ;
#930 = CARTESIAN_POINT ( 'NONE',  ( 39.92123440845005433, 99.26049967264873430, 29.95742577749336988 ) ) ;
#931 = CARTESIAN_POINT ( 'NONE',  ( 43.01140435219951286, 112.4604996726487514, 39.21067981925356349 ) ) ;
#932 = VECTOR ( 'NONE', #17024, 1000.000000000000227 ) ;
#933 = CARTESIAN_POINT ( 'NONE',  ( -159.5594255724347761, -188.7891397928654555, 43.77915905869157598 ) ) ;
#934 = CARTESIAN_POINT ( 'NONE',  ( 47.05648932407426344, 73.91049967264873999, 37.14960608071593384 ) ) ;
#935 = DIRECTION ( 'NONE',  ( 1.000000000000000000, 0.000000000000000000, 0.000000000000000000 ) ) ;
#936 = CARTESIAN_POINT ( 'NONE',  ( -161.4692556286853176, -160.5630981290892976, 49.65701158161630957 ) ) ;
#937 = APPLICATION_PROTOCOL_DEFINITION ( 'draft international standard', 'automotive_design', 1998, #11543 ) ;
#938 = CARTESIAN_POINT ( 'NONE',  ( 43.01140435219951286, 132.5344580088725479, 39.46799094044489209 ) ) ;
#939 = CARTESIAN_POINT ( 'NONE',  ( 43.01140435219951286, 103.1297705074272955, 38.86567161673127657 ) ) ;
#940 = CARTESIAN_POINT ( 'NONE',  ( 40.78231060393920870, 91.71360054188218669, 6.509252002934985626 ) ) ;
#941 = CARTESIAN_POINT ( 'NONE',  ( -148.5561028927606344, -194.7938272943107449, 40.69124936498395328 ) ) ;
#942 = CARTESIAN_POINT ( 'NONE',  ( 39.42975644700377558, 99.41518717409400097, 36.81289934271958941 ) ) ;
#943 = CYLINDRICAL_SURFACE ( 'NONE', #4707, 10.00000000000000888 ) ;
#944 = ORIENTED_EDGE ( 'NONE', *, *, #13725, .T. ) ;
#945 = CARTESIAN_POINT ( 'NONE',  ( 38.01140435219952707, 87.86049967264872862, 35.83527830041809636 ) ) ;
#946 = CARTESIAN_POINT ( 'NONE',  ( 57.14511974427749408, 88.72838517433189054, 6.862995836283489304 ) ) ;
#947 = CIRCLE ( 'NONE', #8357, 10.00000000000000888 ) ;
#948 = CARTESIAN_POINT ( 'NONE',  ( 16.70103016558074316, 129.9804388327498827, 16.57432765154378629 ) ) ;
#949 = CARTESIAN_POINT ( 'NONE',  ( 26.28921445626723852, 149.7786157371718616, -3.732453678475698311 ) ) ;
#950 = CARTESIAN_POINT ( 'NONE',  ( 39.42975644700377558, 81.07977050742731251, 31.60846029578754468 ) ) ;
#951 = VERTEX_POINT ( 'NONE', #1744 ) ;
#952 = ORIENTED_EDGE ( 'NONE', *, *, #905, .F. ) ;
#953 = CARTESIAN_POINT ( 'NONE',  ( 47.43856463449117200, 155.0297705074273154, 32.77220824515698183 ) ) ;
#954 =( BOUNDED_CURVE ( )  B_SPLINE_CURVE ( 2, ( #7542, #12488, #482, #12377, #10736, #21095, #17438, #15682, #5541, #5870, #19215, #16001, #12704 ),
 .UNSPECIFIED., .F., .F. ) 
 B_SPLINE_CURVE_WITH_KNOTS ( ( 3, 2, 2, 2, 2, 2, 3 ),
 ( 0.7321428571428572063, 0.7357142857142857650, 0.7428571428571428825, 0.7500000000000000000, 0.7571428571428571175, 0.7642857142857142350, 0.7678571428571427937 ),
 .UNSPECIFIED. ) 
 CURVE ( )  GEOMETRIC_REPRESENTATION_ITEM ( )  RATIONAL_B_SPLINE_CURVE ( ( 0.9755282581475768211, 0.9755282581475771542, 1.000000000000000000, 0.9510565162951535312, 1.000000000000000000, 0.9510565162951535312, 1.000000000000000000, 0.9510565162951535312, 1.000000000000000000, 0.9510565162951535312, 1.000000000000000000, 0.9755282581475771542, 0.9755282581475768211 ) ) 
 REPRESENTATION_ITEM ( '' )  );
#955 = CARTESIAN_POINT ( 'NONE',  ( -134.9004869860375777, 755.4811543468929358, -19.99999999999996092 ) ) ;
#956 = CIRCLE ( 'NONE', #2372, 5.425037101889737201 ) ;
#957 = CARTESIAN_POINT ( 'NONE',  ( 48.01140435219951996, 119.0604996726487315, 35.83527830041810347 ) ) ;
#959 = CARTESIAN_POINT ( 'NONE',  ( 47.07528247981900904, 85.99676402675389397, -5.799316066731655006 ) ) ;
#958 = CARTESIAN_POINT ( 'NONE',  ( 41.64333658814960870, 80.51518717409400949, 30.00020018409699318 ) ) ;
#960 = CARTESIAN_POINT ( 'NONE',  ( -160.8964159109769696, -166.7438272943107336, 52.72008163687743121 ) ) ;
#961 = CARTESIAN_POINT ( 'NONE',  ( 31.47436479266152531, 87.67613096727390598, 14.72005176623422606 ) ) ;
#962 = CARTESIAN_POINT ( 'NONE',  ( -161.4692556286852607, -184.4130981290893203, 52.90620854394536821 ) ) ;
#963 = SHAPE_REPRESENTATION_RELATIONSHIP ( 'NONE' , 'NONE' ,  #3970, #16628 ) ;
#964 = CYLINDRICAL_SURFACE ( 'NONE', #11411, 10.00000000000000888 ) ;
#966 = ADVANCED_FACE ( 'NONE', ( #3402 ), #18495, .T. ) ;
#965 = DIRECTION ( 'NONE',  ( 0.000000000000000000, -1.000000000000000000, 0.000000000000000000 ) ) ;
#967 = CARTESIAN_POINT ( 'NONE',  ( 45.74753988029933538, 146.3297705074273267, 30.44471234641811819 ) ) ;
#968 = CARTESIAN_POINT ( 'NONE',  ( 75.01029411920679024, 107.5147569559006655, 5.001370044594233732 ) ) ;
#969 = CARTESIAN_POINT ( 'NONE',  ( 39.42975644700377558, 128.8151871740940067, 31.60846029578754468 ) ) ;
#970 = FILL_AREA_STYLE ('',( #2836 ) ) ;
#971 = CARTESIAN_POINT ( 'NONE',  ( -142.0420953463936087, -159.6584106276440593, 49.65701158161630957 ) ) ;
#972 = CARTESIAN_POINT ( 'NONE',  ( 39.42975644700377558, 60.07977050742731251, 31.60846029578754468 ) ) ;
#973 = CARTESIAN_POINT ( 'NONE',  ( 156.5548063637509415, 177.1359029563629406, -29.99999999999997868 ) ) ;
#974 = CARTESIAN_POINT ( 'NONE',  ( 70.54646159239726444, 126.3605644061445901, 18.41388650843374464 ) ) ;
#975 = AXIS2_PLACEMENT_3D ( 'NONE', #5264, #5469, #6716 ) ;
#976 = DIRECTION ( 'NONE',  ( 0.000000000000000000, 1.000000000000000000, 0.000000000000000000 ) ) ;
#977 = CARTESIAN_POINT ( 'NONE',  ( 38.58424406990784661, 105.2651871740939953, 35.64915139335016647 ) ) ;
#978 = EDGE_LOOP ( 'NONE', ( #18658, #5825, #7797, #16450 ) ) ;
#979 = VECTOR ( 'NONE', #11785, 1000.000000000000227 ) ;
#980 = EDGE_CURVE ( 'NONE', #32, #12851, #19907, .T. ) ;
#981 = CARTESIAN_POINT ( 'NONE',  ( -145.2889157411863437, -156.5391397928654555, 41.15050349809589392 ) ) ;
#982 = ORIENTED_EDGE ( 'NONE', *, *, #5579, .F. ) ;
#983 = CARTESIAN_POINT ( 'NONE',  ( 48.01140435219951996, 94.43445800887256780, 32.58608133808903773 ) ) ;
#984 = CARTESIAN_POINT ( 'NONE',  ( 96.62434152388762243, 220.7958015105191976, 4.000000000000021316 ) ) ;
#985 = CARTESIAN_POINT ( 'NONE',  ( 48.01140435219951996, 146.3604996726487570, 32.58608133808903773 ) ) ;
#987 = CARTESIAN_POINT ( 'NONE',  ( 68.32201692705490359, 132.1587870917933003, -0.8393580998851425390 ) ) ;
#986 = CARTESIAN_POINT ( 'NONE',  ( 43.01140435219951286, 107.3651871740940038, 29.55568802177586463 ) ) ;
#988 = EDGE_CURVE ( 'NONE', #1240, #17720, #90, .T. ) ;
#989 = CARTESIAN_POINT ( 'NONE',  ( 38.96631938032478359, 66.41049967264873999, 31.27175355779120025 ) ) ;
#991 = FACE_OUTER_BOUND ( 'NONE', #14368, .T. ) ;
#990 = CARTESIAN_POINT ( 'NONE',  ( 46.98099381664906815, 144.5901365555967004, 37.25520735466820810 ) ) ;
#992 = PRESENTATION_STYLE_ASSIGNMENT (( #9054 ) ) ;
#993 = CARTESIAN_POINT ( 'NONE',  ( 44.55648932407425633, 78.68445800887258201, 38.96596240072933170 ) ) ;
#994 = CARTESIAN_POINT ( 'NONE',  ( 43.01140435219951286, 146.9604996726487229, 29.21067981925356705 ) ) ;
#995 = CARTESIAN_POINT ( 'NONE',  ( 38.58424406990784661, 72.26518717409398107, 35.64915139335016647 ) ) ;
#996 = CARTESIAN_POINT ( 'NONE',  ( 23.17700876947760591, 147.8092992330439586, -3.851376987104358829 ) ) ;
#997 = ADVANCED_FACE ( 'NONE', ( #1851 ), #5796, .T. ) ;
#998 = CARTESIAN_POINT ( 'NONE',  ( 44.55648932407425633, 95.81049967264873146, 29.45539723777780239 ) ) ;
#999 = CARTESIAN_POINT ( 'NONE',  ( -159.0959885057557983, -167.1938272943107222, 44.11586579668791330 ) ) ;
#1000 = CARTESIAN_POINT ( 'NONE',  ( -145.6429501568359797, -181.1084106276440195, 57.67623309621197336 ) ) ;
#1001 = EDGE_LOOP ( 'NONE', ( #7950, #11263, #15363, #5851 ) ) ;
#1002 = CARTESIAN_POINT ( 'NONE',  ( -142.0420953463935803, -171.5084106276440536, 46.59394152635518793 ) ) ;
#1003 = CARTESIAN_POINT ( 'NONE',  ( 73.37616494982036386, 135.8902282719419077, 4.049127002338204662 ) ) ;
#1004 = EDGE_CURVE ( 'NONE', #1468, #11797, #19255, .T. ) ;
#1005 = DIRECTION ( 'NONE',  ( 0.000000000000000000, 0.000000000000000000, -1.000000000000000000 ) ) ;
#1006 = CARTESIAN_POINT ( 'NONE',  ( 46.59305225739526435, 133.3151871740940067, 36.81289934271958941 ) ) ;
#1007 = CARTESIAN_POINT ( 'NONE',  ( 46.59305225739526435, 157.3151871740940067, 36.81289934271958941 ) ) ;
#1008 = CARTESIAN_POINT ( 'NONE',  ( 43.01140435219951286, 98.62977050742730967, 29.55568802177586107 ) ) ;
#1009 = ORIENTED_EDGE ( 'NONE', *, *, #12907, .T. ) ;
#1010 = ORIENTED_EDGE ( 'NONE', *, *, #20723, .T. ) ;
#1011 = EDGE_CURVE ( 'NONE', #20985, #18246, #14067, .T. ) ;
#1012 = CARTESIAN_POINT ( 'NONE',  ( 33.52710748945926866, 93.34978808121778115, 14.79936193957723312 ) ) ;
#1013 = VERTEX_POINT ( 'NONE', #10774 ) ;
#1014 = CARTESIAN_POINT ( 'NONE',  ( 43.01140435219951286, 87.53445800887257633, 39.21067981925356349 ) ) ;
#1015 = EDGE_CURVE ( 'NONE', #4150, #16205, #1153, .T. ) ;
#1016 = CARTESIAN_POINT ( 'NONE',  ( 39.42975644700377558, 75.07977050742731251, 31.60846029578754468 ) ) ;
#1017 = CARTESIAN_POINT ( 'NONE',  ( 47.43856463449118621, 133.6151871740940180, 34.21067981925357060 ) ) ;
#1018 = CARTESIAN_POINT ( 'NONE',  ( 46.10157429594899270, 88.76049967264870588, 38.46393386101376421 ) ) ;
#1019 = CARTESIAN_POINT ( 'NONE',  ( 71.03835150376274044, 100.2492380157770526, 6.267546321443639989 ) ) ;
#1020 = CARTESIAN_POINT ( 'NONE',  ( -143.9637021292202235, -116.9891397928655010, 36.65701158161628825 ) ) ;
#1021 = CARTESIAN_POINT ( 'NONE',  ( -148.3790856849358306, -156.3891397928654783, 40.14644641866477315 ) ) ;
#1022 = CARTESIAN_POINT ( 'NONE',  ( -55.11860757350579831, 784.8075632535900468, -3.999999999999996447 ) ) ;
#1023 = CARTESIAN_POINT ( 'NONE',  ( 116.9721770337685740, 133.1239846058259388, -19.99999999999999289 ) ) ;
#1024 = CARTESIAN_POINT ( 'NONE',  ( 44.55648932407425633, 62.81049967264873146, 29.45539723777780239 ) ) ;
#1025 = ORIENTED_EDGE ( 'NONE', *, *, #8453, .F. ) ;
#1026 = CARTESIAN_POINT ( 'NONE',  ( 46.59305225739526435, 73.57977050742732672, 36.81289934271958941 ) ) ;
#1027 = CARTESIAN_POINT ( 'NONE',  ( -154.3824083646099439, -158.4938272943107052, 40.69124936498395328 ) ) ;
#1028 = CARTESIAN_POINT ( 'NONE',  ( 57.94507594753278568, 150.7106492751291569, -2.660852849641732298 ) ) ;
#1029 = FACE_OUTER_BOUND ( 'NONE', #6208, .T. ) ;
#1030 = VERTEX_POINT ( 'NONE', #5472 ) ;
#1031 = DIRECTION ( 'NONE',  ( -0.000000000000000000, -0.000000000000000000, -1.000000000000000000 ) ) ;
#1032 = AXIS2_PLACEMENT_3D ( 'NONE', #6238, #19694, #16478 ) ;
#1033 = CARTESIAN_POINT ( 'NONE',  ( 48.01140435219951996, 124.1344580088725706, 35.83527830041809636 ) ) ;
#1034 = CARTESIAN_POINT ( 'NONE',  ( 46.59305225739526435, 121.5797705074273267, 36.81289934271958941 ) ) ;
#1035 = ORIENTED_EDGE ( 'NONE', *, *, #7465, .F. ) ;
#1036 = ADVANCED_FACE ( 'NONE', ( #2390 ), #7256, .F. ) ;
#1037 = CARTESIAN_POINT ( 'NONE',  ( 43.80332655382220253, 129.6113394311928460, 39.21067981925355639 ) ) ;
#1038 = ORIENTED_EDGE ( 'NONE', *, *, #10703, .F. ) ;
#1039 = CARTESIAN_POINT ( 'NONE',  ( 44.37947211624943833, 128.4797705074273040, 30.00020018409699318 ) ) ;
#1040 = CARTESIAN_POINT ( 'NONE',  ( -154.5594255724347761, -155.1630981290892919, 40.14644641866476604 ) ) ;
#1041 = CARTESIAN_POINT ( 'NONE',  ( 48.01140435219951996, 64.13445800887257064, 35.83527830041810347 ) ) ;
#1042 = STYLED_ITEM ( 'NONE', ( #2053 ), #21529 ) ;
#1043 = FACE_OUTER_BOUND ( 'NONE', #2864, .T. ) ;
#1044 = CARTESIAN_POINT ( 'NONE',  ( 161.4773229304660731, 84.89323405393692212, 4.000000000000021316 ) ) ;
#1045 =( LENGTH_UNIT ( ) NAMED_UNIT ( * ) SI_UNIT ( .MILLI., .METRE. ) );
#1046 = CARTESIAN_POINT ( 'NONE',  ( -154.5594255724347761, -186.0891397928654953, 40.14644641866476604 ) ) ;
#1047 = CARTESIAN_POINT ( 'NONE',  ( 43.80332655382220253, 73.53738109496899256, 39.21067981925355639 ) ) ;
#1048 = CARTESIAN_POINT ( 'NONE',  ( 44.55648932407425633, 94.88445800887257064, 29.45539723777780239 ) ) ;
#1049 = CARTESIAN_POINT ( 'NONE',  ( -148.5561028927606344, -194.7938272943107449, 40.69124936498395328 ) ) ;
#1050 = CARTESIAN_POINT ( 'NONE',  ( 43.01140435219951286, 135.5344580088726048, 39.46799094044489209 ) ) ;
#1051 = CARTESIAN_POINT ( 'NONE',  ( 45.74753988029933538, 104.3297705074272983, 30.44471234641811819 ) ) ;
#1052 = CARTESIAN_POINT ( 'NONE',  ( 34.49559591455799534, 146.8750064778945728, 2.580435534661669195 ) ) ;
#1053 = DIRECTION ( 'NONE',  ( 0.000000000000000000, 1.000000000000000000, 0.000000000000000000 ) ) ;
#1054 = CARTESIAN_POINT ( 'NONE',  ( 47.43856463449118621, 97.61518717409400381, 34.21067981925357060 ) ) ;
#1055 = DIRECTION ( 'NONE',  ( -1.000000000000000000, 0.000000000000000000, 0.000000000000000000 ) ) ;
#1056 = VERTEX_POINT ( 'NONE', #12418 ) ;
#1057 = CARTESIAN_POINT ( 'NONE',  ( 147.5268905834513475, 193.0332408774651185, -50.99999999999998579 ) ) ;
#1058 = CARTESIAN_POINT ( 'NONE',  ( 54.54805624998882507, 152.1374805055981199, -2.779977617235711129 ) ) ;
#1059 = CARTESIAN_POINT ( 'NONE',  ( 47.43856463449117911, 146.0297705074272869, 32.77220824515697473 ) ) ;
#1060 = CARTESIAN_POINT ( 'NONE',  ( 43.85786119575681852, 148.0137586191354444, -9.053472026759274982 ) ) ;
#1061 = ADVANCED_FACE ( 'NONE', ( #2071, #9126 ), #20695, .F. ) ;
#1062 = CARTESIAN_POINT ( 'NONE',  ( 23.67598417054553295, 91.65793073385727041, -5.994147020910363999 ) ) ;
#1063 = AXIS2_PLACEMENT_3D ( 'NONE', #15504, #3927, #12404 ) ;
#1064 = CARTESIAN_POINT ( 'NONE',  ( 46.59305225739526435, 64.57977050742731251, 36.81289934271958941 ) ) ;
#1065 = EDGE_LOOP ( 'NONE', ( #5086, #8694, #5474, #2167 ) ) ;
#1066 = ORIENTED_EDGE ( 'NONE', *, *, #4103, .F. ) ;
#1067 = CARTESIAN_POINT ( 'NONE',  ( 40.27526882409969033, 152.9297705074273210, 30.44471234641811819 ) ) ;
#1068 = FACE_OUTER_BOUND ( 'NONE', #16645, .T. ) ;
#1069 = ADVANCED_FACE ( 'NONE', ( #8909 ), #19146, .F. ) ;
#1070 = CARTESIAN_POINT ( 'NONE',  ( 46.10157429594899270, 124.7604996726487485, 38.46393386101376421 ) ) ;
#1072 = CARTESIAN_POINT ( 'NONE',  ( 8.922311181598237440, 122.0085103898528018, 10.15299703236346573 ) ) ;
#1071 = CARTESIAN_POINT ( 'NONE',  ( 43.01140435219951286, 74.36518717409400381, 29.55568802177586463 ) ) ;
#1073 = CARTESIAN_POINT ( 'NONE',  ( -154.3824083646099439, -155.7584106276440536, 40.69124936498395328 ) ) ;
#1074 = CARTESIAN_POINT ( 'NONE',  ( -142.0420953463936087, -168.3938272943107393, 49.65701158161630957 ) ) ;
#1075 = CARTESIAN_POINT ( 'NONE',  ( 72.33162239183086228, 137.5781058455011703, 11.98183203572534872 ) ) ;
#1076 = CARTESIAN_POINT ( 'NONE',  ( -143.3790856849358306, -188.7630981290893146, 43.77915905869157598 ) ) ;
#1077 = PLANE ( 'NONE',  #8255 ) ;
#1078 = DIRECTION ( 'NONE',  ( 0.000000000000000000, 1.000000000000000000, 0.000000000000000000 ) ) ;
#1079 = CARTESIAN_POINT ( 'NONE',  ( 38.58424406990784661, 129.2297705074273324, 32.77220824515698183 ) ) ;
#1080 = CARTESIAN_POINT ( 'NONE',  ( 43.59077634914400079, 154.2158251336064723, 2.858602931426994953 ) ) ;
#1081 = CARTESIAN_POINT ( 'NONE',  ( 47.43856463449117911, 124.7651871740940095, 32.77220824515697473 ) ) ;
#1082 = CARTESIAN_POINT ( 'NONE',  ( 38.96631938032478359, 69.41049967264873999, 31.27175355779120025 ) ) ;
#1083 = CARTESIAN_POINT ( 'NONE',  ( 43.01140435219951996, 149.9604996726487798, 29.21067981925357060 ) ) ;
#1084 = CARTESIAN_POINT ( 'NONE',  ( 44.55648932407425633, 139.6104996726487286, 38.96596240072933170 ) ) ;
#1085 = CARTESIAN_POINT ( 'NONE',  ( -120.0322075325610598, -126.9891397928655010, -54.65701158161630246 ) ) ;
#1086 = CARTESIAN_POINT ( 'NONE',  ( 58.78870511939484800, 143.3781512503299780, 17.58070913143554748 ) ) ;
#1087 = CARTESIAN_POINT ( 'NONE',  ( 43.01140435219951286, 83.96049967264873715, 29.21067981925356705 ) ) ;
#1088 = CARTESIAN_POINT ( 'NONE',  ( 40.27526882409969033, 105.5651871740939782, 37.97664729208901946 ) ) ;
#1089 =( BOUNDED_CURVE ( )  B_SPLINE_CURVE ( 2, ( #9097, #10319, #12063, #10425, #15488, #389, #7118, #15798, #13610, #17021, #1929, #12166, #10533 ),
 .UNSPECIFIED., .F., .F. ) 
 B_SPLINE_CURVE_WITH_KNOTS ( ( 3, 2, 2, 2, 2, 2, 3 ),
 ( 0.3602941176470588203, 0.3617647058823529327, 0.3647058823529411575, 0.3676470588235294379, 0.3705882352941176627, 0.3735294117647058876, 0.3750000000000000000 ),
 .UNSPECIFIED. ) 
 CURVE ( )  GEOMETRIC_REPRESENTATION_ITEM ( )  RATIONAL_B_SPLINE_CURVE ( ( 0.9755282581475768211, 0.9755282581475768211, 1.000000000000000000, 0.9510565162951535312, 1.000000000000000000, 0.9510565162951535312, 1.000000000000000000, 0.9510565162951535312, 1.000000000000000000, 0.9510565162951535312, 1.000000000000000000, 0.9755282581475768211, 0.9755282581475768211 ) ) 
 REPRESENTATION_ITEM ( '' )  );
#1090 = ORIENTED_EDGE ( 'NONE', *, *, #12786, .T. ) ;
#1091 = PLANE ( 'NONE',  #19799 ) ;
#1092 = ADVANCED_FACE ( 'NONE', ( #10668 ), #19042, .T. ) ;
#1093 = ORIENTED_EDGE ( 'NONE', *, *, #6809, .T. ) ;
#1094 = CARTESIAN_POINT ( 'NONE',  ( 48.01140435219951996, 94.13445800887258486, 35.83527830041810347 ) ) ;
#1095 = CARTESIAN_POINT ( 'NONE',  ( 38.96631938032478359, 151.0104996726487343, 37.14960608071593384 ) ) ;
#1097 = CARTESIAN_POINT ( 'NONE',  ( 37.89917375590665927, 147.5588116854153498, -9.291614562240097186 ) ) ;
#1096 = CARTESIAN_POINT ( 'NONE',  ( 44.37947211624943833, 110.2151871740940123, 30.00020018409699318 ) ) ;
#1099 = CARTESIAN_POINT ( 'NONE',  ( -151.4692556286852607, -183.8130981290892692, 59.65701158161632378 ) ) ;
#1098 = CARTESIAN_POINT ( 'NONE',  ( 43.66945230930459587, 144.9005013971865594, 39.17809732472422013 ) ) ;
#1100 = DIRECTION ( 'NONE',  ( 0.000000000000000000, 0.000000000000000000, 1.000000000000000000 ) ) ;
#1101 = LINE ( 'NONE', #19613, #20236 ) ;
#1102 = CARTESIAN_POINT ( 'NONE',  ( 109.8528842077358405, 344.7014318495014322, 4.000000000000003553 ) ) ;
#1103 = CARTESIAN_POINT ( 'NONE',  ( 38.58424406990784661, 59.96518717409398391, 32.77220824515698183 ) ) ;
#1104 = CARTESIAN_POINT ( 'NONE',  ( 23.67598417054553295, 91.65793073385727041, -5.994147020910363999 ) ) ;
#1105 = CARTESIAN_POINT ( 'NONE',  ( 40.27526882409969744, 152.6651871740940010, 30.44471234641812174 ) ) ;
#1106 = CARTESIAN_POINT ( 'NONE',  ( 43.01140435219951286, 113.9604996726487371, 29.21067981925356705 ) ) ;
#1107 = CARTESIAN_POINT ( 'NONE',  ( -151.4692556286852891, -170.6438272943107677, 39.74470866294723947 ) ) ;
#1108 = CARTESIAN_POINT ( 'NONE',  ( -159.0959885057557983, -185.4584106276440707, 44.11586579668791330 ) ) ;
#1109 = ORIENTED_EDGE ( 'NONE', *, *, #17157, .T. ) ;
#1110 = CARTESIAN_POINT ( 'NONE',  ( 38.58424406990786082, 72.11518717409400381, 34.21067981925357060 ) ) ;
#1111 = CARTESIAN_POINT ( 'NONE',  ( -151.4692556286852891, -173.9084106276440593, 39.74470866294723947 ) ) ;
#1112 = CARTESIAN_POINT ( 'NONE',  ( 41.39294982251618649, 154.1830292177732531, 16.78735015533800734 ) ) ;
#1113 = SURFACE_STYLE_USAGE ( .BOTH. , #16419 ) ;
#1114 = CARTESIAN_POINT ( 'NONE',  ( 43.01140435219951286, 131.3651871740940180, 29.55568802177586463 ) ) ;
#1115 = ADVANCED_FACE ( 'NONE', ( #520 ), #15825, .T. ) ;
#1116 = VERTEX_POINT ( 'NONE', #18932 ) ;
#1117 = EDGE_LOOP ( 'NONE', ( #9478, #7959, #7011, #10296 ) ) ;
#1118 = VECTOR ( 'NONE', #4322, 1000.000000000000000 ) ;
#1119 = CARTESIAN_POINT ( 'NONE',  ( 25.64412274706724304, 97.69032544021251852, 15.15625305551708202 ) ) ;
#1120 = ORIENTED_EDGE ( 'NONE', *, *, #3662, .F. ) ;
#1121 = CARTESIAN_POINT ( 'NONE',  ( 38.01140435219952707, 116.7844580088725763, 34.21067981925357060 ) ) ;
#1122 = LINE ( 'NONE', #12914, #6565 ) ;
#1123 = VECTOR ( 'NONE', #20357, 1000.000000000000000 ) ;
#1124 = CARTESIAN_POINT ( 'NONE',  ( 47.43856463449117200, 79.72977050742728977, 35.64915139335016647 ) ) ;
#1125 = CARTESIAN_POINT ( 'NONE',  ( 43.01140435219951286, 137.3651871740940180, 29.55568802177586463 ) ) ;
#1126 = CARTESIAN_POINT ( 'NONE',  ( 39.92123440845004723, 94.16049967264871157, 38.46393386101376421 ) ) ;
#1127 = CARTESIAN_POINT ( 'NONE',  ( 40.90832812944997698, 154.0758954209757121, 3.767805038447253452 ) ) ;
#1128 = CARTESIAN_POINT ( 'NONE',  ( 40.50225576765475921, 95.03178743630938641, 38.54804764342390655 ) ) ;
#1129 = CARTESIAN_POINT ( 'NONE',  ( -157.6495955161842062, -158.0391397928654271, 58.16351966513671812 ) ) ;
#1130 = CARTESIAN_POINT ( 'NONE',  ( 46.10157429594899270, 151.7344580088725934, 29.95742577749336988 ) ) ;
#1131 = CARTESIAN_POINT ( 'NONE',  ( -176.9699209214867608, -126.9891397928655010, -35.00000000000000000 ) ) ;
#1132 = VECTOR ( 'NONE', #18955, 1000.000000000000114 ) ;
#1133 = ORIENTED_EDGE ( 'NONE', *, *, #15104, .F. ) ;
#1134 = CARTESIAN_POINT ( 'NONE',  ( 47.43856463449118621, 70.87977050742732388, 34.21067981925357060 ) ) ;
#1135 = CARTESIAN_POINT ( 'NONE',  ( -157.2955611005346270, -193.7084106276440423, 57.67623309621198047 ) ) ;
#1136 = CARTESIAN_POINT ( 'NONE',  ( 69.83118287335672392, 141.1824132108841638, 4.838974892866481525 ) ) ;
#1137 = CARTESIAN_POINT ( 'NONE',  ( -160.8964159109769696, -188.1584106276440593, 49.65701158161630957 ) ) ;
#1138 = VERTEX_POINT ( 'NONE', #9014 ) ;
#1139 = DIRECTION ( 'NONE',  ( -1.233581138472395521E-15, -0.000000000000000000, 1.000000000000000000 ) ) ;
#1140 = CARTESIAN_POINT ( 'NONE',  ( 48.01140435219951996, 124.4344580088725678, 32.58608133808903773 ) ) ;
#1141 = ADVANCED_FACE ( 'NONE', ( #15726 ), #629, .T. ) ;
#1142 = CARTESIAN_POINT ( 'NONE',  ( 39.42975644700377558, 123.6797705074273210, 36.81289934271958941 ) ) ;
#1143 = ORIENTED_EDGE ( 'NONE', *, *, #9526, .F. ) ;
#1144 = FACE_OUTER_BOUND ( 'NONE', #21457, .T. ) ;
#1145 = ORIENTED_EDGE ( 'NONE', *, *, #15285, .F. ) ;
#1146 = CARTESIAN_POINT ( 'NONE',  ( 43.01140435219951286, 127.1297705074273381, 38.86567161673127657 ) ) ;
#1147 = CARTESIAN_POINT ( 'NONE',  ( 45.51140435220141001, 58.78519719078001060, 29.88055280033245964 ) ) ;
#1148 = CARTESIAN_POINT ( 'NONE',  ( 41.46631938032478359, 60.38445800887257064, 38.96596240072933170 ) ) ;
#1149 = DIRECTION ( 'NONE',  ( 0.5010362705417042983, 0.000000000000000000, 0.8654262854811264338 ) ) ;
#1150 = CARTESIAN_POINT ( 'NONE',  ( 38.96631938032478359, 101.4844580088725792, 31.27175355779120025 ) ) ;
#1151 = CARTESIAN_POINT ( 'NONE',  ( -157.6495955161842062, -176.0391397928654555, 58.16351966513671812 ) ) ;
#1152 = CARTESIAN_POINT ( 'NONE',  ( -151.4692556286852891, -184.7391397928654442, 60.17163382399899518 ) ) ;
#1153 =( BOUNDED_CURVE ( )  B_SPLINE_CURVE ( 2, ( #10559, #8800, #5578, #10982, #14279, #12302, #3832, #2171, #9234, #20910, #21025, #3938, #5907 ),
 .UNSPECIFIED., .F., .F. ) 
 B_SPLINE_CURVE_WITH_KNOTS ( ( 3, 2, 2, 2, 2, 2, 3 ),
 ( 0.6250000000000000000, 0.6285714285714285587, 0.6357142857142856762, 0.6428571428571429047, 0.6500000000000000222, 0.6571428571428571397, 0.6607142857142856984 ),
 .UNSPECIFIED. ) 
 CURVE ( )  GEOMETRIC_REPRESENTATION_ITEM ( )  RATIONAL_B_SPLINE_CURVE ( ( 0.9755282581475768211, 0.9755282581475768211, 1.000000000000000000, 0.9510565162951535312, 1.000000000000000000, 0.9510565162951535312, 1.000000000000000000, 0.9510565162951535312, 1.000000000000000000, 0.9510565162951535312, 1.000000000000000000, 0.9755282581475768211, 0.9755282581475768211 ) ) 
 REPRESENTATION_ITEM ( '' )  );
#1154 = CARTESIAN_POINT ( 'NONE',  ( 38.01140435219952707, 89.63445800887258486, 32.58608133808903773 ) ) ;
#1155 = CARTESIAN_POINT ( 'NONE',  ( 47.05648932407426344, 130.9104996726487684, 37.14960608071593384 ) ) ;
#1156 = CARTESIAN_POINT ( 'NONE',  ( -148.5561028927606344, -185.7938272943107449, 40.69124936498395328 ) ) ;
#1157 = SHAPE_DEFINITION_REPRESENTATION ( #11328, #17468 ) ;
#1158 = EDGE_CURVE ( 'NONE', #8610, #10777, #21440, .T. ) ;
#1159 = CARTESIAN_POINT ( 'NONE',  ( 44.55648932407425633, 126.6844580088725678, 38.96596240072933170 ) ) ;
#1160 = CARTESIAN_POINT ( 'NONE',  ( 43.01140435219951286, 101.6297705074273239, 29.55568802177586463 ) ) ;
#1161 = CARTESIAN_POINT ( 'NONE',  ( 39.55749537675153960, 91.83829536962669238, 20.55682687220188143 ) ) ;
#1162 = CARTESIAN_POINT ( 'NONE',  ( -151.4692556286852891, -185.6438272943107393, 39.74470866294723947 ) ) ;
#1163 = CARTESIAN_POINT ( 'NONE',  ( 41.64333658814960870, 99.71518717409399812, 38.42115945441014446 ) ) ;
#1164 = DIRECTION ( 'NONE',  ( 0.000000000000000000, 1.000000000000000000, 0.000000000000000000 ) ) ;
#1165 = ORIENTED_EDGE ( 'NONE', *, *, #14487, .T. ) ;
#1166 = CARTESIAN_POINT ( 'NONE',  ( 43.80332655382220253, 127.5373810949690068, 39.21067981925355639 ) ) ;
#1167 = CARTESIAN_POINT ( 'NONE',  ( 47.47886434171987702, 153.8471147930492862, -3.017879606865911502 ) ) ;
#1168 = CARTESIAN_POINT ( 'NONE',  ( 68.06566224877710169, 132.6756899087416457, -7.863043133634088910 ) ) ;
#1169 = CARTESIAN_POINT ( 'NONE',  ( 43.01140435219951286, 64.12977050742730967, 38.86567161673127657 ) ) ;
#1170 = ORIENTED_EDGE ( 'NONE', *, *, #12310, .T. ) ;
#1171 = ORIENTED_EDGE ( 'NONE', *, *, #13365, .T. ) ;
#1172 = CARTESIAN_POINT ( 'NONE',  ( 47.43856463449118621, 157.8797705074273381, 34.21067981925357060 ) ) ;
#1173 = CARTESIAN_POINT ( 'NONE',  ( -56.84366818088135176, 789.5005544000622422, -3.999999999999996447 ) ) ;
#1174 = CARTESIAN_POINT ( 'NONE',  ( 41.46631938032478359, 109.3104996726487457, 38.96596240072933170 ) ) ;
#1176 = CARTESIAN_POINT ( 'NONE',  ( 56.11190468687431832, 151.4478768383145280, 5.272225788895710252 ) ) ;
#1175 = CARTESIAN_POINT ( 'NONE',  ( 45.74753988029933538, 70.16518717409397254, 37.97664729208901946 ) ) ;
#1177 = CARTESIAN_POINT ( 'NONE',  ( -142.0420953463935803, -156.5084106276439968, 46.59394152635518793 ) ) ;
#1178 = CARTESIAN_POINT ( 'NONE',  ( -160.8964159109769696, -169.7438272943107052, 52.72008163687743121 ) ) ;
#1179 = DIRECTION ( 'NONE',  ( -0.000000000000000000, -0.000000000000000000, -1.000000000000000000 ) ) ;
#1180 = CARTESIAN_POINT ( 'NONE',  ( -161.4692556286852607, -181.7130981290892464, 46.40781461928724383 ) ) ;
#1181 = EDGE_CURVE ( 'NONE', #11596, #5848, #13724, .T. ) ;
#1182 = FACE_OUTER_BOUND ( 'NONE', #1117, .T. ) ;
#1183 = CARTESIAN_POINT ( 'NONE',  ( 47.05648932407426344, 148.5844580088725877, 31.27175355779120025 ) ) ;
#1184 = CARTESIAN_POINT ( 'NONE',  ( 43.01140435219951286, 133.1297705074273381, 38.86567161673127657 ) ) ;
#1185 = CARTESIAN_POINT ( 'NONE',  ( 9.585575214713108139, 112.1464265272871188, 0.8345760063739874335 ) ) ;
#1186 = CARTESIAN_POINT ( 'NONE',  ( 40.27526882409969744, 122.6651871740939725, 30.44471234641812174 ) ) ;
#1187 = CARTESIAN_POINT ( 'NONE',  ( -151.4692556286852891, -126.9891397928655010, 39.65701158161630246 ) ) ;
#1188 = CARTESIAN_POINT ( 'NONE',  ( -151.4692556286852891, -155.9084106276440593, 39.74470866294723947 ) ) ;
#1189 = CARTESIAN_POINT ( 'NONE',  ( 48.01140435219951996, 65.06049967264873146, 35.83527830041809636 ) ) ;
#1190 = PLANE ( 'NONE',  #6786 ) ;
#1191 = CARTESIAN_POINT ( 'NONE',  ( 66.16974147772015158, 135.9983230778657344, -9.010293137571032673 ) ) ;
#1192 = DIRECTION ( 'NONE',  ( 1.000000000000000000, 0.000000000000000000, 0.000000000000000000 ) ) ;
#1193 = VERTEX_POINT ( 'NONE', #2609 ) ;
#1194 = DIRECTION ( 'NONE',  ( 1.000000000000000000, 0.000000000000000000, 0.000000000000000000 ) ) ;
#1195 = VERTEX_POINT ( 'NONE', #9025 ) ;
#1196 = CARTESIAN_POINT ( 'NONE',  ( 43.01140435219951286, 84.53445800887256212, 39.46799094044489209 ) ) ;
#1197 = LINE ( 'NONE', #6263, #13695 ) ;
#1198 = CARTESIAN_POINT ( 'NONE',  ( 43.01140435219951286, 151.4604996726486945, 39.46799094044489209 ) ) ;
#1200 = CARTESIAN_POINT ( 'NONE',  ( 48.12388674207330297, 92.25590008057444891, 8.208355790051324874 ) ) ;
#1199 = CARTESIAN_POINT ( 'NONE',  ( 38.58424406990784661, 95.96518717409396970, 32.77220824515698183 ) ) ;
#1201 = CARTESIAN_POINT ( 'NONE',  ( -160.8964159109769696, -164.3084106276440650, 46.59394152635518793 ) ) ;
#1202 = EDGE_CURVE ( 'NONE', #15353, #21725, #13833, .T. ) ;
#1203 = CARTESIAN_POINT ( 'NONE',  ( 46.10157429594899270, 64.76049967264873430, 38.46393386101376421 ) ) ;
#1205 = FACE_OUTER_BOUND ( 'NONE', #8630, .T. ) ;
#1204 = CARTESIAN_POINT ( 'NONE',  ( 47.85046472749336743, 144.4343633168767269, 32.91075569967801329 ) ) ;
#1206 = CARTESIAN_POINT ( 'NONE',  ( 43.01140435219951286, 104.9604996726487371, 29.21067981925356705 ) ) ;
#1207 = CARTESIAN_POINT ( 'NONE',  ( 43.01140435219951286, 78.53445800887259054, 39.21067981925356349 ) ) ;
#1208 = CARTESIAN_POINT ( 'NONE',  ( -176.9699209214867892, 72.84679049016736485, -25.00000000000000000 ) ) ;
#1209 = CARTESIAN_POINT ( 'NONE',  ( 40.27526882409969033, 59.66518717409400097, 30.44471234641811819 ) ) ;
#1210 = FACE_OUTER_BOUND ( 'NONE', #15224, .T. ) ;
#1211 = VECTOR ( 'NONE', #3473, 1000.000000000000000 ) ;
#1212 = CARTESIAN_POINT ( 'NONE',  ( 47.43856463449117911, 151.4651871740939839, 35.64915139335015937 ) ) ;
#1213 = CARTESIAN_POINT ( 'NONE',  ( 38.96631938032478359, 114.4104996726487400, 31.27175355779120025 ) ) ;
#1214 = CARTESIAN_POINT ( 'NONE',  ( -159.0959885057557983, -172.5938272943107279, 55.19815736654470584 ) ) ;
#1215 = CARTESIAN_POINT ( 'NONE',  ( -143.8425227516148084, -189.3584106276440480, 44.11586579668791330 ) ) ;
#1216 = ORIENTED_EDGE ( 'NONE', *, *, #20304, .F. ) ;
#1217 = CARTESIAN_POINT ( 'NONE',  ( 46.59305225739526435, 64.91518717409400097, 31.60846029578754468 ) ) ;
#1218 =( BOUNDED_CURVE ( )  B_SPLINE_CURVE ( 2, ( #11812, #15004, #3449, #13140, #2997, #1458, #19987, #9736, #16657, #9842, #14785, #16768, #6653 ),
 .UNSPECIFIED., .F., .F. ) 
 B_SPLINE_CURVE_WITH_KNOTS ( ( 3, 2, 2, 2, 2, 2, 3 ),
 ( 0.1985294117647058987, 0.2000000000000000111, 0.2029411764705882359, 0.2058823529411764608, 0.2088235294117647134, 0.2117647058823529382, 0.2132352941176470507 ),
 .UNSPECIFIED. ) 
 CURVE ( )  GEOMETRIC_REPRESENTATION_ITEM ( )  RATIONAL_B_SPLINE_CURVE ( ( 0.9755282581475768211, 0.9755282581475770431, 1.000000000000000000, 0.9510565162951535312, 1.000000000000000000, 0.9510565162951535312, 1.000000000000000000, 0.9510565162951535312, 1.000000000000000000, 0.9510565162951535312, 1.000000000000000000, 0.9755282581475768211, 0.9755282581475768211 ) ) 
 REPRESENTATION_ITEM ( '' )  );
#1219 = CARTESIAN_POINT ( 'NONE',  ( -142.0420953463935803, -165.5084106276439968, 46.59394152635518793 ) ) ;
#1220 = CARTESIAN_POINT ( 'NONE',  ( 10.76517401744387215, 131.6399553617083029, 15.47769843104460463 ) ) ;
#1221 = CARTESIAN_POINT ( 'NONE',  ( 47.05648932407426344, 111.9844580088725792, 37.14960608071593384 ) ) ;
#1222 = CARTESIAN_POINT ( 'NONE',  ( 43.01140435219951286, 137.3651871740940180, 29.55568802177586463 ) ) ;
#1223 = CARTESIAN_POINT ( 'NONE',  ( 9.504183449854689769, 113.2927979568517571, -4.132695447411913747 ) ) ;
#1224 = ORIENTED_EDGE ( 'NONE', *, *, #1690, .F. ) ;
#1225 = ORIENTED_EDGE ( 'NONE', *, *, #2133, .T. ) ;
#1226 = CARTESIAN_POINT ( 'NONE',  ( 14.85320491933239317, 121.4429315054255909, 16.22795414098078126 ) ) ;
#1227 = VERTEX_POINT ( 'NONE', #4367 ) ;
#1228 = CYLINDRICAL_SURFACE ( 'NONE', #10090, 4.999999999999997335 ) ;
#1230 = CARTESIAN_POINT ( 'NONE',  ( 15.00983914341701997, 123.2415857317943448, 2.299110145932334426 ) ) ;
#1229 = CARTESIAN_POINT ( 'NONE',  ( 47.43856463449118621, 136.6151871740940180, 34.21067981925357060 ) ) ;
#1231 = CARTESIAN_POINT ( 'NONE',  ( 43.01140435219951286, 86.96049967264873715, 28.95336869806222779 ) ) ;
#1232 = CARTESIAN_POINT ( 'NONE',  ( 65.27013532398795803, 145.9152199903044504, 11.62486143609835310 ) ) ;
#1233 = DIRECTION ( 'NONE',  ( 1.000000000000000000, 0.000000000000000000, 0.000000000000000000 ) ) ;
#1234 = CARTESIAN_POINT ( 'NONE',  ( -154.5594255724347761, -163.8891397928654499, 59.16757674456785310 ) ) ;
#1235 = CARTESIAN_POINT ( 'NONE',  ( 45.74753988029933538, 89.06518717409399244, 30.44471234641811819 ) ) ;
#1236 = CARTESIAN_POINT ( 'NONE',  ( 48.01140435219951996, 107.2104996726487371, 34.21067981925357060 ) ) ;
#1237 = CARTESIAN_POINT ( 'NONE',  ( 148.6725454929228079, -61.68114226949890622, 19.99999999999998934 ) ) ;
#1238 = CARTESIAN_POINT ( 'NONE',  ( 43.80332655382220253, 142.9575765865523351, 29.21067981925356705 ) ) ;
#1239 = EDGE_CURVE ( 'NONE', #13557, #19772, #12755, .T. ) ;
#1240 = VERTEX_POINT ( 'NONE', #21355 ) ;
#1241 = CARTESIAN_POINT ( 'NONE',  ( 38.58424406990784661, 78.22977050742731819, 32.77220824515698183 ) ) ;
#1242 = CARTESIAN_POINT ( 'NONE',  ( -143.8425227516148084, -192.3584106276440480, 44.11586579668791330 ) ) ;
#1243 = CARTESIAN_POINT ( 'NONE',  ( 26.90790578767411390, 150.1165885900122987, 3.291480155758420345 ) ) ;
#1244 = CARTESIAN_POINT ( 'NONE',  ( -159.0959885057557983, -182.4584106276440707, 44.11586579668791330 ) ) ;
#1245 = EDGE_LOOP ( 'NONE', ( #6658, #5520, #15881, #12747 ) ) ;
#1246 = DIRECTION ( 'NONE',  ( -0.3450121214752274734, 0.9385982292947089300, 0.000000000000000000 ) ) ;
#1247 = FACE_OUTER_BOUND ( 'NONE', #20004, .T. ) ;
#1248 = CARTESIAN_POINT ( 'NONE',  ( 45.74753988029934249, 121.4297705074273210, 37.97664729208901235 ) ) ;
#1249 = VERTEX_POINT ( 'NONE', #14943 ) ;
#1250 = CARTESIAN_POINT ( 'NONE',  ( -151.4692556286852891, -185.3130981290893260, 39.65701158161630246 ) ) ;
#1251 = ORIENTED_EDGE ( 'NONE', *, *, #15611, .F. ) ;
#1252 = CARTESIAN_POINT ( 'NONE',  ( 45.74753988029933538, 115.4297705074272926, 37.97664729208901946 ) ) ;
#1253 = DIRECTION ( 'NONE',  ( -0.9599098561846887145, -0.2803088796301151375, 0.000000000000000000 ) ) ;
#1254 = EDGE_CURVE ( 'NONE', #5159, #8610, #16077, .T. ) ;
#1255 = CARTESIAN_POINT ( 'NONE',  ( 41.46631938032478359, 62.18445800887258201, 29.45539723777780239 ) ) ;
#1256 = EDGE_CURVE ( 'NONE', #2768, #6341, #16602, .T. ) ;
#1257 = CYLINDRICAL_SURFACE ( 'NONE', #244, 5.000000000000004441 ) ;
#1258 = LINE ( 'NONE', #14373, #6793 ) ;
#1259 = CARTESIAN_POINT ( 'NONE',  ( 38.01140435219952707, 96.71049967264875136, 34.21067981925357060 ) ) ;
#1260 = CARTESIAN_POINT ( 'NONE',  ( -161.4692556286853176, -191.4891397928654726, 49.65701158161630957 ) ) ;
#1261 = EDGE_CURVE ( 'NONE', #872, #17856, #18371, .T. ) ;
#1262 = CARTESIAN_POINT ( 'NONE',  ( -151.4692556286852891, -196.9891397928655010, 39.65701158161630246 ) ) ;
#1263 = CARTESIAN_POINT ( 'NONE',  ( 38.01140435219952707, 102.7104996726487514, 34.21067981925357060 ) ) ;
#1264 = CARTESIAN_POINT ( 'NONE',  ( -148.5561028927606344, -188.7938272943107449, 40.69124936498395328 ) ) ;
#1265 = ITEM_DEFINED_TRANSFORMATION ( 'NONE', 'NONE', #19717,  #12657 ) ;
#1266 = AXIS2_PLACEMENT_3D ( 'NONE', #2104, #12019, #2214 ) ;
#1267 = CARTESIAN_POINT ( 'NONE',  ( 38.01140435219951996, 119.9344580088725678, 35.83527830041810347 ) ) ;
#1268 = CARTESIAN_POINT ( 'NONE',  ( 38.58424406990784661, 102.2297705074273182, 32.77220824515698183 ) ) ;
#1269 = CARTESIAN_POINT ( 'NONE',  ( 69.69253243162556544, 129.2828754355126648, 18.29472124897268159 ) ) ;
#1270 = CARTESIAN_POINT ( 'NONE',  ( -142.0420953463935803, -180.5438272943106881, 52.72008163687743831 ) ) ;
#1271 = CARTESIAN_POINT ( 'NONE',  ( 47.43856463449118621, 85.61518717409400381, 34.21067981925357060 ) ) ;
#1272 = EDGE_CURVE ( 'NONE', #951, #12140, #21577, .T. ) ;
#1273 = CARTESIAN_POINT ( 'NONE',  ( 43.01140435219951996, 10.71049967264875491, 34.21067981925357060 ) ) ;
#1274 = ORIENTED_EDGE ( 'NONE', *, *, #9783, .F. ) ;
#1275 = CARTESIAN_POINT ( 'NONE',  ( 48.01140435219951996, 128.2104996726487514, 34.21067981925357060 ) ) ;
#1276 = CARTESIAN_POINT ( 'NONE',  ( 63.41425016244589585, 92.41789933959738335, 6.624947895572852019 ) ) ;
#1277 = CARTESIAN_POINT ( 'NONE',  ( 69.05514009256096131, 130.5101840208823205, -14.76775785107876082 ) ) ;
#1278 = CARTESIAN_POINT ( 'NONE',  ( 44.37947211624943833, 67.27977050742731535, 38.42115945441014446 ) ) ;
#1279 = ORIENTED_EDGE ( 'NONE', *, *, #10623, .F. ) ;
#1280 = ORIENTED_EDGE ( 'NONE', *, *, #9639, .T. ) ;
#1281 = CARTESIAN_POINT ( 'NONE',  ( 41.64333658814960870, 152.7797705074273438, 30.00020018409699318 ) ) ;
#1282 = EDGE_CURVE ( 'NONE', #4009, #10043, #14611, .T. ) ;
#1283 = AXIS2_PLACEMENT_3D ( 'NONE', #5031, #8562, #5245 ) ;
#1284 = DIRECTION ( 'NONE',  ( 0.000000000000000000, 1.000000000000000000, 0.000000000000000000 ) ) ;
#1285 = EDGE_CURVE ( 'NONE', #17073, #9338, #6245, .T. ) ;
#1286 = CARTESIAN_POINT ( 'NONE',  ( 48.01140435219951996, 107.3604996726487428, 32.58608133808903773 ) ) ;
#1287 = CARTESIAN_POINT ( 'NONE',  ( 47.43856463449117200, 67.46518717409399812, 35.64915139335016647 ) ) ;
#1288 = CARTESIAN_POINT ( 'NONE',  ( 38.96631938032478359, 66.08445800887258770, 37.14960608071593384 ) ) ;
#1289 = CARTESIAN_POINT ( 'NONE',  ( -154.3824083646099439, -161.4938272943107336, 40.69124936498395328 ) ) ;
#1290 = CARTESIAN_POINT ( 'NONE',  ( 42.21948215057684450, 156.4575765865523351, 39.21067981925356349 ) ) ;
#1291 = CARTESIAN_POINT ( 'NONE',  ( -154.5594255724347761, -174.9630981290893033, 59.16757674456785310 ) ) ;
#1292 = CARTESIAN_POINT ( 'NONE',  ( 47.05648932407426344, 150.9844580088725934, 37.14960608071593384 ) ) ;
#1293 = CARTESIAN_POINT ( 'NONE',  ( 41.64333658814960870, 128.7797705074273438, 30.00020018409699318 ) ) ;
#1294 = CARTESIAN_POINT ( 'NONE',  ( 26.67903320394502131, 150.0857490671680807, 9.287084330314211655 ) ) ;
#1295 = AXIS2_PLACEMENT_3D ( 'NONE', #8946, #12021, #2108 ) ;
#1296 = CARTESIAN_POINT ( 'NONE',  ( 43.01140435219951286, 125.3651871740939896, 29.55568802177586107 ) ) ;
#1297 = CARTESIAN_POINT ( 'NONE',  ( -153.0531000319306827, -168.1622583705451746, 39.65701158161629536 ) ) ;
#1298 = CARTESIAN_POINT ( 'NONE',  ( 38.01140435219952707, 150.8604996726487570, 35.83527830041809636 ) ) ;
#1299 = DIRECTION ( 'NONE',  ( 0.000000000000000000, 1.000000000000000000, 0.000000000000000000 ) ) ;
#1300 = CARTESIAN_POINT ( 'NONE',  ( 0.08333186253067781379, 634.6318465664365931, -19.99999999999997868 ) ) ;
#1301 = CARTESIAN_POINT ( 'NONE',  ( 59.92122946415073415, 142.4742691614619332, -9.367183195626855863 ) ) ;
#1302 = DIRECTION ( 'NONE',  ( 0.000000000000000000, -1.000000000000000000, 0.000000000000000000 ) ) ;
#1303 = VERTEX_POINT ( 'NONE', #3051 ) ;
#1304 = CARTESIAN_POINT ( 'NONE',  ( 43.01140435219951996, 119.9070776186055838, -35.00000000000000000 ) ) ;
#1305 = VERTEX_POINT ( 'NONE', #9789 ) ;
#1306 = CARTESIAN_POINT ( 'NONE',  ( 41.46631938032478359, 86.18445800887256780, 29.45539723777780239 ) ) ;
#1307 = FACE_OUTER_BOUND ( 'NONE', #18026, .T. ) ;
#1308 = VECTOR ( 'NONE', #20782, 1000.000000000000000 ) ;
#1309 = CARTESIAN_POINT ( 'NONE',  ( 48.01140435219951996, 137.0604996726487457, 35.83527830041810347 ) ) ;
#1311 = CARTESIAN_POINT ( 'NONE',  ( 33.24893159794274311, 146.2783277815063059, 4.518043653832040540 ) ) ;
#1310 = CARTESIAN_POINT ( 'NONE',  ( 40.27526882409969033, 96.56518717409399244, 37.97664729208901946 ) ) ;
#1312 = DIRECTION ( 'NONE',  ( 0.000000000000000000, 0.000000000000000000, 1.000000000000000000 ) ) ;
#1313 = CARTESIAN_POINT ( 'NONE',  ( -157.2955611005346270, -166.7084106276440423, 57.67623309621198047 ) ) ;
#1314 = CARTESIAN_POINT ( 'NONE',  ( -160.8964159109769696, -187.8938272943107393, 49.65701158161630957 ) ) ;
#1316 = CARTESIAN_POINT ( 'NONE',  ( 18.67254549292281496, -61.68114226949890622, -16.21320343559643717 ) ) ;
#1315 = DIRECTION ( 'NONE',  ( -0.3450121214752274179, 0.9385982292947088190, -0.000000000000000000 ) ) ;
#1317 = CARTESIAN_POINT ( 'NONE',  ( -141.4692556286852891, -189.2130981290893317, 52.90620854394536821 ) ) ;
#1318 = CARTESIAN_POINT ( 'NONE',  ( -148.3790856849358306, -174.3891397928654783, 40.14644641866477315 ) ) ;
#1319 = CARTESIAN_POINT ( 'NONE',  ( 48.01140435219951996, 80.21049967264875136, 34.21067981925357060 ) ) ;
#1320 = CARTESIAN_POINT ( 'NONE',  ( 38.58424406990784661, 62.96518717409399812, 32.77220824515698183 ) ) ;
#1321 = CARTESIAN_POINT ( 'NONE',  ( 46.60148787037231699, 85.86292235506145687, 7.220022382731924537 ) ) ;
#1322 = VECTOR ( 'NONE', #10602, 1000.000000000000000 ) ;
#1323 = CARTESIAN_POINT ( 'NONE',  ( -142.0420953463936087, -165.3938272943107393, 49.65701158161630957 ) ) ;
#1324 = CARTESIAN_POINT ( 'NONE',  ( -148.5561028927606344, -184.2584106276440536, 58.62277379824867296 ) ) ;
#1325 = ORIENTED_EDGE ( 'NONE', *, *, #18533, .F. ) ;
#1326 = CARTESIAN_POINT ( 'NONE',  ( 43.01140435219951286, 72.86518717409400381, 38.86567161673127657 ) ) ;
#1327 = CARTESIAN_POINT ( 'NONE',  ( -159.0959885057557983, -173.4584106276440423, 44.11586579668791330 ) ) ;
#1328 = CARTESIAN_POINT ( 'NONE',  ( 63.06653971011325410, 92.06373373134326243, 19.64449301269484849 ) ) ;
#1329 = CIRCLE ( 'NONE', #8736, 24.99999999999999289 ) ;
#1330 = CARTESIAN_POINT ( 'NONE',  ( 43.80332655382220253, 112.9575765865522925, 29.21067981925356705 ) ) ;
#1331 = CARTESIAN_POINT ( 'NONE',  ( 45.74753988029933538, 133.1651871740940010, 37.97664729208901946 ) ) ;
#1332 = CARTESIAN_POINT ( 'NONE',  ( 15.69291839309778958, 99.40984958608130739, -11.63272432674803802 ) ) ;
#1333 = ORIENTED_EDGE ( 'NONE', *, *, #2207, .T. ) ;
#1334 = VERTEX_POINT ( 'NONE', #19922 ) ;
#1335 = ADVANCED_FACE ( 'NONE', ( #16484 ), #1400, .F. ) ;
#1336 = CARTESIAN_POINT ( 'NONE',  ( 44.86974823489592978, 148.0457227541334362, 10.98970740178311090 ) ) ;
#1337 = VERTEX_POINT ( 'NONE', #14617 ) ;
#1338 = FACE_OUTER_BOUND ( 'NONE', #2820, .T. ) ;
#1339 = CARTESIAN_POINT ( 'NONE',  ( 47.43856463449117200, 67.72977050742731819, 35.64915139335016647 ) ) ;
#1341 = CARTESIAN_POINT ( 'NONE',  ( 17.20459894546975832, 108.5405110446994001, 1.704077971530460811 ) ) ;
#1340 = CARTESIAN_POINT ( 'NONE',  ( 39.42975644700377558, 128.8151871740940067, 31.60846029578754468 ) ) ;
#1342 = AXIS2_PLACEMENT_3D ( 'NONE', #8297, #20202, #15234 ) ;
#1343 = CARTESIAN_POINT ( 'NONE',  ( 48.01140435219951996, 92.36049967264871441, 32.58608133808903773 ) ) ;
#1344 = DIRECTION ( 'NONE',  ( -0.000000000000000000, 1.000000000000000000, 0.000000000000000000 ) ) ;
#1345 = CARTESIAN_POINT ( 'NONE',  ( 41.71169011715027608, 94.93878194014966709, 29.37128083581765381 ) ) ;
#1346 = CARTESIAN_POINT ( 'NONE',  ( -156.4692864601533131, -155.0638355923473455, 40.99677534440144200 ) ) ;
#1347 =( BOUNDED_CURVE ( )  B_SPLINE_CURVE ( 2, ( #695, #14130, #5757, #4111, #5868, #12598, #19319, #4217, #10947, #16956, #16516, #8496, #1868 ),
 .UNSPECIFIED., .F., .F. ) 
 B_SPLINE_CURVE_WITH_KNOTS ( ( 3, 2, 2, 2, 2, 2, 3 ),
 ( 0.007352941176470590735, 0.008823529411764705760, 0.01176470588235294101, 0.01470588235294117627, 0.01764705882352941152, 0.02058823529411764677, 0.02205882352941176267 ),
 .UNSPECIFIED. ) 
 CURVE ( )  GEOMETRIC_REPRESENTATION_ITEM ( )  RATIONAL_B_SPLINE_CURVE ( ( 0.9755282581475768211, 0.9755282581475768211, 1.000000000000000000, 0.9510565162951535312, 1.000000000000000000, 0.9510565162951535312, 1.000000000000000000, 0.9510565162951535312, 1.000000000000000000, 0.9510565162951535312, 1.000000000000000000, 0.9755282581475768211, 0.9755282581475768211 ) ) 
 REPRESENTATION_ITEM ( '' )  );
#1348 = CARTESIAN_POINT ( 'NONE',  ( 43.01140435219951286, 90.86518717409400381, 38.86567161673127657 ) ) ;
#1349 = EDGE_CURVE ( 'NONE', #2985, #4126, #2691, .T. ) ;
#1350 = LINE ( 'NONE', #11046, #6604 ) ;
#1351 = DIRECTION ( 'NONE',  ( -0.000000000000000000, 1.000000000000000000, -0.000000000000000000 ) ) ;
#1352 = ORIENTED_EDGE ( 'NONE', *, *, #661, .T. ) ;
#1353 = CARTESIAN_POINT ( 'NONE',  ( 38.58424406990784661, 78.52977050742730114, 35.64915139335016647 ) ) ;
#1354 = CARTESIAN_POINT ( 'NONE',  ( -157.2955611005346270, -158.3438272943106995, 41.63779006702063867 ) ) ;
#1355 = CARTESIAN_POINT ( 'NONE',  ( 26.13368487350976110, 90.12329638092472806, 0.9106621812756837686 ) ) ;
#1356 = CARTESIAN_POINT ( 'NONE',  ( -151.4692556286852891, -181.4084106276440025, 59.56931450028537967 ) ) ;
#1357 = ORIENTED_EDGE ( 'NONE', *, *, #19930, .F. ) ;
#1358 = CARTESIAN_POINT ( 'NONE',  ( -151.4692556286852607, -162.2391397928654442, 39.65701158161629536 ) ) ;
#1359 = LINE ( 'NONE', #8090, #5000 ) ;
#1360 = CARTESIAN_POINT ( 'NONE',  ( 38.58424406990786082, 123.3797705074273239, 34.21067981925357060 ) ) ;
#1361 = ORIENTED_EDGE ( 'NONE', *, *, #10597, .F. ) ;
#1362 = CARTESIAN_POINT ( 'NONE',  ( 46.10157429594899270, 129.8344580088725877, 38.46393386101375711 ) ) ;
#1363 = ORIENTED_EDGE ( 'NONE', *, *, #15641, .T. ) ;
#1364 = CARTESIAN_POINT ( 'NONE',  ( 44.37947211624943833, 121.2797705074273296, 38.42115945441014446 ) ) ;
#1365 = CARTESIAN_POINT ( 'NONE',  ( 44.37947211624943833, 154.0151871740940237, 38.42115945441014446 ) ) ;
#1366 = EDGE_CURVE ( 'NONE', #10070, #12769, #541, .T. ) ;
#1367 = CARTESIAN_POINT ( 'NONE',  ( -156.4692594822809610, -155.3725178653323553, 40.99675976862926063 ) ) ;
#1368 = CARTESIAN_POINT ( 'NONE',  ( 38.01140435219952707, 83.63445800887258486, 32.58608133808903773 ) ) ;
#1369 =( NAMED_UNIT ( * ) PLANE_ANGLE_UNIT ( ) SI_UNIT ( $, .RADIAN. ) );
#1370 = CARTESIAN_POINT ( 'NONE',  ( -154.5594255724347761, -187.8891397928654783, 59.16757674456785310 ) ) ;
#1371 = LINE ( 'NONE', #8103, #10134 ) ;
#1372 = FACE_OUTER_BOUND ( 'NONE', #14553, .T. ) ;
#1373 = PRODUCT_RELATED_PRODUCT_CATEGORY ( 'part', '', ( #8687 ) ) ;
#1374 = CARTESIAN_POINT ( 'NONE',  ( -154.3824083646099439, -191.4938272943107336, 40.69124936498395328 ) ) ;
#1375 = APPLICATION_PROTOCOL_DEFINITION ( 'draft international standard', 'automotive_design', 1998, #15053 ) ;
#1376 = AXIS2_PLACEMENT_3D ( 'NONE', #4360, #21349, #17699 ) ;
#1377 = CARTESIAN_POINT ( 'NONE',  ( 41.46631938032478359, 128.1844580088725820, 29.45539723777780239 ) ) ;
#1378 = CARTESIAN_POINT ( 'NONE',  ( 40.27526882409969033, 102.8297705074272983, 37.97664729208901946 ) ) ;
#1379 = CARTESIAN_POINT ( 'NONE',  ( 26.70363248220801466, 142.8423586596025245, -10.77201286955609127 ) ) ;
#1380 = CARTESIAN_POINT ( 'NONE',  ( -151.4692556286852891, -179.6438272943107393, 39.74470866294723947 ) ) ;
#1381 = CARTESIAN_POINT ( 'NONE',  ( 45.74753988029934249, 85.16518717409400097, 37.97664729208901235 ) ) ;
#1382 = CARTESIAN_POINT ( 'NONE',  ( -158.9748091281504401, -126.9891397928655010, 36.65701158161628115 ) ) ;
#1383 = ORIENTED_EDGE ( 'NONE', *, *, #20635, .T. ) ;
#1384 = CARTESIAN_POINT ( 'NONE',  ( 48.01140435219951996, 128.3604996726487286, 32.58608133808903773 ) ) ;
#1385 = CARTESIAN_POINT ( 'NONE',  ( 16.30372524420941716, 141.3216567370616019, 9.839263250375132941 ) ) ;
#1386 = EDGE_CURVE ( 'NONE', #6341, #2204, #8241, .T. ) ;
#1387 = CARTESIAN_POINT ( 'NONE',  ( 46.59305225739526435, 146.1797705074273495, 31.60846029578754468 ) ) ;
#1388 = CARTESIAN_POINT ( 'NONE',  ( 40.25662930883660806, 147.8909896968035014, -16.19631701608006580 ) ) ;
#1389 = CARTESIAN_POINT ( 'NONE',  ( 43.01140435219951286, 62.62977050742732388, 29.55568802177586107 ) ) ;
#1390 = ORIENTED_EDGE ( 'NONE', *, *, #18659, .T. ) ;
#1391 = EDGE_CURVE ( 'NONE', #3863, #16834, #3608, .T. ) ;
#1392 = ORIENTED_EDGE ( 'NONE', *, *, #20409, .F. ) ;
#1393 = CARTESIAN_POINT ( 'NONE',  ( 38.58424406990784661, 150.5297705074272869, 35.64915139335016647 ) ) ;
#1394 = VECTOR ( 'NONE', #2475, 1000.000000000000000 ) ;
#1395 = CYLINDRICAL_SURFACE ( 'NONE', #20750, 14.42424326798555434 ) ;
#1396 = CARTESIAN_POINT ( 'NONE',  ( 47.05648932407426344, 109.9104996726487400, 37.14960608071593384 ) ) ;
#1397 = CARTESIAN_POINT ( 'NONE',  ( 40.27526882409969033, 66.56518717409400665, 37.97664729208901946 ) ) ;
#1398 = CARTESIAN_POINT ( 'NONE',  ( 41.46631938032478359, 95.18445800887258201, 29.45539723777780239 ) ) ;
#1399 = CARTESIAN_POINT ( 'NONE',  ( -148.5561028927606344, -158.7938272943107449, 40.69124936498395328 ) ) ;
#1400 = CYLINDRICAL_SURFACE ( 'NONE', #21320, 13.99821153497579651 ) ;
#1401 = CARTESIAN_POINT ( 'NONE',  ( -141.4692556286852891, -183.2130981290892748, 52.90620854394536821 ) ) ;
#1402 = DIRECTION ( 'NONE',  ( 0.000000000000000000, 1.000000000000000000, 0.000000000000000000 ) ) ;
#1403 = CARTESIAN_POINT ( 'NONE',  ( 48.01140435219951996, 151.4344580088725820, 32.58608133808903773 ) ) ;
#1404 = CARTESIAN_POINT ( 'NONE',  ( 44.37947211624943833, 130.2797705074273154, 38.42115945441014446 ) ) ;
#1405 = CARTESIAN_POINT ( 'NONE',  ( 62.21295035458982881, 148.3457431455455549, 17.50134052088148096 ) ) ;
#1406 = CARTESIAN_POINT ( 'NONE',  ( 45.74753988029934249, 115.1651871740940010, 37.97664729208901235 ) ) ;
#1407 = CARTESIAN_POINT ( 'NONE',  ( -161.4692556286852891, -167.6391397928654499, 46.40781461928724383 ) ) ;
#1408 = DIRECTION ( 'NONE',  ( 0.000000000000000000, -1.000000000000000000, 0.000000000000000000 ) ) ;
#1409 = APPLICATION_CONTEXT ( 'automotive_design' ) ;
#1410 = PRODUCT_DEFINITION_FORMATION_WITH_SPECIFIED_SOURCE ( 'ANY', '', #14993, .NOT_KNOWN. ) ;
#1411 = CARTESIAN_POINT ( 'NONE',  ( 43.01140435219950575, 139.4604996726487514, 39.21067981925356349 ) ) ;
#1412 = CARTESIAN_POINT ( 'NONE',  ( 24.63684302007652249, 148.6959638282970957, 4.200683933265449532 ) ) ;
#1413 = CARTESIAN_POINT ( 'NONE',  ( 69.04633063039527485, 130.7408809369782716, -8.772150750671475095 ) ) ;
#1414 = CARTESIAN_POINT ( 'NONE',  ( 47.05648932407426344, 82.91049967264873999, 37.14960608071593384 ) ) ;
#1415 = CARTESIAN_POINT ( 'NONE',  ( 43.01140435219951286, 91.12977050742732388, 38.86567161673127657 ) ) ;
#1416 = EDGE_LOOP ( 'NONE', ( #13580, #12610, #16747, #17987 ) ) ;
#1417 = CARTESIAN_POINT ( 'NONE',  ( -136.4581486297550441, -126.9891397928655010, 49.65701158161631668 ) ) ;
#1418 = ORIENTED_EDGE ( 'NONE', *, *, #7944, .F. ) ;
#1419 = CARTESIAN_POINT ( 'NONE',  ( 46.10157429594899270, 84.83445800887258770, 38.46393386101376421 ) ) ;
#1420 = CARTESIAN_POINT ( 'NONE',  ( 137.5268905834513191, 193.0332408774651185, -29.99999999999997868 ) ) ;
#1421 = CARTESIAN_POINT ( 'NONE',  ( 38.01140435219951996, 138.8604996726487286, 35.83527830041810347 ) ) ;
#1423 = CARTESIAN_POINT ( 'NONE',  ( 15.29689364450883815, 124.6620785063593786, 10.35143954082134954 ) ) ;
#1422 = CARTESIAN_POINT ( 'NONE',  ( 47.43856463449118621, 97.61518717409400381, 34.21067981925357060 ) ) ;
#1424 = CARTESIAN_POINT ( 'NONE',  ( 147.5268905834513475, 193.0332408774651185, -5.999999999999976019 ) ) ;
#1425 = CARTESIAN_POINT ( 'NONE',  ( -160.8964159109769696, -170.1584106276440593, 49.65701158161630957 ) ) ;
#1426 = CARTESIAN_POINT ( 'NONE',  ( -154.3824083646099439, -188.4938272943107336, 40.69124936498395328 ) ) ;
#1428 = CYLINDRICAL_SURFACE ( 'NONE', #9034, 7.500000000000000000 ) ;
#1427 = CARTESIAN_POINT ( 'NONE',  ( -157.6495955161842062, -167.0130981290893146, 41.15050349809589392 ) ) ;
#1429 = DIRECTION ( 'NONE',  ( 0.000000000000000000, 0.000000000000000000, -1.000000000000000000 ) ) ;
#1430 = DIRECTION ( 'NONE',  ( 0.000000000000000000, 1.000000000000000000, 0.000000000000000000 ) ) ;
#1431 = LINE ( 'NONE', #10574, #2685 ) ;
#1432 = CARTESIAN_POINT ( 'NONE',  ( 47.43856463449117200, 158.0297705074273438, 32.77220824515698183 ) ) ;
#1433 = CARTESIAN_POINT ( 'NONE',  ( 67.39040179371399120, 143.9404232637865562, 4.720051584306741432 ) ) ;
#1434 = CARTESIAN_POINT ( 'NONE',  ( 38.58424406990786082, 144.1151871740939896, 34.21067981925357060 ) ) ;
#1435 = CARTESIAN_POINT ( 'NONE',  ( -160.8964159109769696, -157.8938272943107393, 49.65701158161630957 ) ) ;
#1436 = CARTESIAN_POINT ( 'NONE',  ( -154.3824083646099439, -184.5584106276440650, 58.62277379824867296 ) ) ;
#1437 = EDGE_CURVE ( 'NONE', #15249, #13513, #20359, .T. ) ;
#1438 = EDGE_CURVE ( 'NONE', #310, #16002, #8512, .T. ) ;
#1439 = ORIENTED_EDGE ( 'NONE', *, *, #1940, .T. ) ;
#1440 = CARTESIAN_POINT ( 'NONE',  ( 45.74753988029934249, 73.16518717409400097, 37.97664729208901235 ) ) ;
#1441 = CARTESIAN_POINT ( 'NONE',  ( -145.6429501568359797, -168.2084106276440139, 41.63779006702063867 ) ) ;
#1442 = CARTESIAN_POINT ( 'NONE',  ( 21.21153947156776809, 146.4065673692475400, 16.07276909216647454 ) ) ;
#1443 = CARTESIAN_POINT ( 'NONE',  ( 129.2454342010813662, 193.1635054290503319, -44.99999999999997158 ) ) ;
#1444 = CARTESIAN_POINT ( 'NONE',  ( 46.59305225739526435, 124.3151871740940067, 36.81289934271958941 ) ) ;
#1445 = AXIS2_PLACEMENT_3D ( 'NONE', #7171, #18740, #10262 ) ;
#1446 = CARTESIAN_POINT ( 'NONE',  ( 13.64837572802379562, 102.4646860582014796, -11.51360178106338594 ) ) ;
#1447 = VERTEX_POINT ( 'NONE', #18595 ) ;
#1448 = ORIENTED_EDGE ( 'NONE', *, *, #20139, .F. ) ;
#1449 = ORIENTED_EDGE ( 'NONE', *, *, #19445, .T. ) ;
#1450 = CARTESIAN_POINT ( 'NONE',  ( 38.01140435219951996, 107.9344580088725536, 35.83527830041810347 ) ) ;
#1451 = CARTESIAN_POINT ( 'NONE',  ( 111.4021762516569964, 137.5714195593754710, -19.99999999999997868 ) ) ;
#1452 = CARTESIAN_POINT ( 'NONE',  ( 44.37947211624943833, 68.47977050742731819, 30.00020018409699318 ) ) ;
#1454 = CARTESIAN_POINT ( 'NONE',  ( 63.07923660420441792, 139.7192868340247571, 4.799362114056002326 ) ) ;
#1453 = CARTESIAN_POINT ( 'NONE',  ( 40.27526882409969033, 125.6651871740939868, 30.44471234641811819 ) ) ;
#1455 = CARTESIAN_POINT ( 'NONE',  ( 38.96631938032478359, 85.01049967264874851, 37.14960608071593384 ) ) ;
#1456 = CARTESIAN_POINT ( 'NONE',  ( 83.67254549292280785, -61.68114226949890622, -16.21320343559643717 ) ) ;
#1457 = CARTESIAN_POINT ( 'NONE',  ( -141.4692556286852891, -171.2130981290893033, 52.90620854394536821 ) ) ;
#1458 = CARTESIAN_POINT ( 'NONE',  ( 38.01140435219952707, 138.8604996726487286, 35.83527830041809636 ) ) ;
#1459 = CARTESIAN_POINT ( 'NONE',  ( 39.42975644700377558, 89.81518717409400665, 31.60846029578754468 ) ) ;
#1460 = CARTESIAN_POINT ( 'NONE',  ( 43.01140435219951286, 156.5344580088725479, 39.21067981925355639 ) ) ;
#1461 = CARTESIAN_POINT ( 'NONE',  ( 77.34521997529867576, 314.8592298662555322, 272.0939500981630204 ) ) ;
#1462 = EDGE_CURVE ( 'NONE', #9423, #12336, #15502, .T. ) ;
#1463 = ORIENTED_EDGE ( 'NONE', *, *, #1366, .F. ) ;
#1464 = CARTESIAN_POINT ( 'NONE',  ( 45.74753988029933538, 65.32977050742732672, 30.44471234641811819 ) ) ;
#1465 = CARTESIAN_POINT ( 'NONE',  ( -148.5561028927606344, -159.9938272943107336, 58.62277379824867296 ) ) ;
#1466 = CARTESIAN_POINT ( 'NONE',  ( 40.90832812944997698, 154.0758954209757121, 3.767805038447253452 ) ) ;
#1467 = CARTESIAN_POINT ( 'NONE',  ( -160.8964159109769696, -185.1584106276440309, 49.65701158161630957 ) ) ;
#1468 = VERTEX_POINT ( 'NONE', #3500 ) ;
#1469 = CARTESIAN_POINT ( 'NONE',  ( 40.27526882409969033, 156.5651871740939498, 37.97664729208901946 ) ) ;
#1470 = CARTESIAN_POINT ( 'NONE',  ( 43.01140435219951996, 10.71049967264875491, 29.21067981925357060 ) ) ;
#1471 = CARTESIAN_POINT ( 'NONE',  ( 40.27526882409969744, 116.9297705074273210, 30.44471234641812174 ) ) ;
#1472 = CARTESIAN_POINT ( 'NONE',  ( 61.61057083318216598, 91.16763906547615193, -7.303593892219363504 ) ) ;
#1473 = ORIENTED_EDGE ( 'NONE', *, *, #15351, .T. ) ;
#1474 = CARTESIAN_POINT ( 'NONE',  ( 46.10157429594899270, 130.7344580088725934, 29.95742577749336988 ) ) ;
#1475 = ORIENTED_EDGE ( 'NONE', *, *, #325, .F. ) ;
#1476 = CARTESIAN_POINT ( 'NONE',  ( 41.64333658814960870, 114.9797705074273324, 38.42115945441014446 ) ) ;
#1477 = CARTESIAN_POINT ( 'NONE',  ( 180.1254907973641934, 54.87273858953557237, 4.000000000000021316 ) ) ;
#1478 = CARTESIAN_POINT ( 'NONE',  ( 38.58424406990784661, 158.9651871740940123, 32.77220824515698183 ) ) ;
#1479 =( BOUNDED_CURVE ( )  B_SPLINE_CURVE ( 2, ( #2640, #9383, #998, #6712, #9497, #14436, #1624, #6163, #7626, #15976, #16194, #17956, #7841 ),
 .UNSPECIFIED., .F., .F. ) 
 B_SPLINE_CURVE_WITH_KNOTS ( ( 3, 2, 2, 2, 2, 2, 3 ),
 ( 0.6250000000000000000, 0.6264705882352941124, 0.6294117647058823373, 0.6323529411764705621, 0.6352941176470587870, 0.6382352941176470118, 0.6397058823529411242 ),
 .UNSPECIFIED. ) 
 CURVE ( )  GEOMETRIC_REPRESENTATION_ITEM ( )  RATIONAL_B_SPLINE_CURVE ( ( 0.9755282581475768211, 0.9755282581475768211, 1.000000000000000000, 0.9510565162951535312, 1.000000000000000000, 0.9510565162951535312, 1.000000000000000000, 0.9510565162951535312, 1.000000000000000000, 0.9510565162951535312, 1.000000000000000000, 0.9755282581475777093, 0.9755282581475768211 ) ) 
 REPRESENTATION_ITEM ( '' )  );
#1480 = AXIS2_PLACEMENT_3D ( 'NONE', #7219, #13919, #14029 ) ;
#1481 = CIRCLE ( 'NONE', #2895, 7.500000000000000000 ) ;
#1482 = DIRECTION ( 'NONE',  ( 0.000000000000000000, 0.000000000000000000, -1.000000000000000000 ) ) ;
#1483 = CARTESIAN_POINT ( 'NONE',  ( 42.21948215057684450, 84.45757658655229250, 39.21067981925355639 ) ) ;
#1484 = CYLINDRICAL_SURFACE ( 'NONE', #8889, 10.00000000000000888 ) ;
#1485 = CARTESIAN_POINT ( 'NONE',  ( -148.3790856849358306, -183.3891397928654783, 40.14644641866477315 ) ) ;
#1486 = CARTESIAN_POINT ( 'NONE',  ( 38.96631938032478359, 90.08445800887257349, 37.14960608071593384 ) ) ;
#1487 = CARTESIAN_POINT ( 'NONE',  ( 43.80332655382222384, 93.61133943119286016, 39.21067981925354928 ) ) ;
#1488 = CARTESIAN_POINT ( 'NONE',  ( -159.0959885057557983, -188.1938272943107222, 44.11586579668791330 ) ) ;
#1489 = ITEM_DEFINED_TRANSFORMATION ( 'NONE', 'NONE', #15826,  #12657 ) ;
#1490 = CARTESIAN_POINT ( 'NONE',  ( 48.01140435219951996, 127.4344580088725962, 32.58608133808903773 ) ) ;
#1491 = CARTESIAN_POINT ( 'NONE',  ( 46.59305225739526435, 95.17977050742732104, 31.60846029578754468 ) ) ;
#1492 = CARTESIAN_POINT ( 'NONE',  ( 19.04663372520828801, 134.9227921665808765, 15.79488502079956547 ) ) ;
#1493 = CARTESIAN_POINT ( 'NONE',  ( -143.8425227516148084, -180.6938272943107506, 55.19815736654470584 ) ) ;
#1494 = CARTESIAN_POINT ( 'NONE',  ( 47.43856463449117911, 88.46518717409399812, 35.64915139335015937 ) ) ;
#1495 = FACE_OUTER_BOUND ( 'NONE', #11432, .T. ) ;
#1496 = EDGE_LOOP ( 'NONE', ( #21649, #1881, #15539, #573, #5295, #13906, #7867, #3916 ) ) ;
#1497 = CARTESIAN_POINT ( 'NONE',  ( 126.8576204525573274, -136.9891397928655010, 67.64809332337412684 ) ) ;
#1498 = CARTESIAN_POINT ( 'NONE',  ( 55.94180145820917716, 151.6039095241057453, 11.26783467880839140 ) ) ;
#1499 = CARTESIAN_POINT ( 'NONE',  ( 47.44511438772692458, 147.6747606579048409, -1.910614883896327054 ) ) ;
#1500 = CARTESIAN_POINT ( 'NONE',  ( 46.59305225739526435, 103.3151871740940067, 36.81289934271958941 ) ) ;
#1501 = PRODUCT ( 'Hinges', 'Hinges', '', ( #2695 ) ) ;
#1502 = CARTESIAN_POINT ( 'NONE',  ( 45.74753988029934249, 68.32977050742732672, 30.44471234641812174 ) ) ;
#1503 = ORIENTED_EDGE ( 'NONE', *, *, #17821, .F. ) ;
#1504 = CARTESIAN_POINT ( 'NONE',  ( 45.74753988029933538, 146.3297705074273267, 30.44471234641811819 ) ) ;
#1505 = CARTESIAN_POINT ( 'NONE',  ( 39.42975644700377558, 99.67977050742732104, 36.81289934271958941 ) ) ;
#1506 = EDGE_CURVE ( 'NONE', #14220, #7040, #17142, .T. ) ;
#1507 = FACE_OUTER_BOUND ( 'NONE', #6778, .T. ) ;
#1508 = CARTESIAN_POINT ( 'NONE',  ( 39.92123440845004723, 106.1604996726487400, 38.46393386101376421 ) ) ;
#1509 = CARTESIAN_POINT ( 'NONE',  ( 41.64333658814960870, 71.51518717409399528, 30.00020018409699318 ) ) ;
#1510 = CARTESIAN_POINT ( 'NONE',  ( 116.9721770337685740, 133.1239846058259388, -35.00000000000000000 ) ) ;
#1511 = CARTESIAN_POINT ( 'NONE',  ( -159.0959885057557983, -157.5938272943107279, 55.19815736654470584 ) ) ;
#1512 = DIRECTION ( 'NONE',  ( 0.000000000000000000, -1.000000000000000000, 0.000000000000000000 ) ) ;
#1513 = CARTESIAN_POINT ( 'NONE',  ( -148.3790856849358306, -182.4630981290893033, 40.14644641866477315 ) ) ;
#1514 = DIRECTION ( 'NONE',  ( 0.000000000000000000, 0.000000000000000000, 1.000000000000000000 ) ) ;
#1515 = CARTESIAN_POINT ( 'NONE',  ( 43.01140435219951286, 147.5344580088725763, 39.46799094044489209 ) ) ;
#1516 = CARTESIAN_POINT ( 'NONE',  ( 39.42975644700377558, 135.6797705074273210, 36.81289934271958941 ) ) ;
#1517 = CARTESIAN_POINT ( 'NONE',  ( 70.82039710638956365, 99.80338443054456832, 19.28708432993385102 ) ) ;
#1518 = CARTESIAN_POINT ( 'NONE',  ( 45.74753988029934249, 121.1651871740939868, 37.97664729208901235 ) ) ;
#1519 = CARTESIAN_POINT ( 'NONE',  ( -161.4692556286852891, -182.6391397928654499, 46.40781461928724383 ) ) ;
#1520 = CARTESIAN_POINT ( 'NONE',  ( -143.9637021292202235, -126.9891397928655010, 36.65701158161628825 ) ) ;
#1521 = CARTESIAN_POINT ( 'NONE',  ( 44.55648932407425633, 64.61049967264874283, 38.96596240072933170 ) ) ;
#1522 = CARTESIAN_POINT ( 'NONE',  ( 59.50342836137831171, 89.99885106877826502, 7.772197353298202493 ) ) ;
#1523 = CARTESIAN_POINT ( 'NONE',  ( 55.20039838223064521, 94.47806301326188816, -0.08174959847185196693 ) ) ;
#1524 = CARTESIAN_POINT ( 'NONE',  ( 41.64333658814960870, 99.97977050742731819, 38.42115945441014446 ) ) ;
#1525 = VERTEX_POINT ( 'NONE', #17247 ) ;
#1526 = CARTESIAN_POINT ( 'NONE',  ( 43.01140435219951286, 146.0344580088725479, 29.21067981925356705 ) ) ;
#1527 = ORIENTED_EDGE ( 'NONE', *, *, #18029, .T. ) ;
#1528 = CARTESIAN_POINT ( 'NONE',  ( 44.55648932407425633, 82.88445800887257064, 29.45539723777780239 ) ) ;
#1529 = CARTESIAN_POINT ( 'NONE',  ( 41.46631938032478359, 86.18445800887256780, 29.45539723777780239 ) ) ;
#1530 = CARTESIAN_POINT ( 'NONE',  ( 44.55648932407425633, 137.8104996726487457, 29.45539723777780239 ) ) ;
#1532 = CARTESIAN_POINT ( 'NONE',  ( 71.12409474721032154, 120.5409021055102841, -0.3630727742139398528 ) ) ;
#1531 = CARTESIAN_POINT ( 'NONE',  ( 44.37947211624943833, 97.01518717409400949, 38.42115945441014446 ) ) ;
#1533 = CARTESIAN_POINT ( 'NONE',  ( -145.6429501568359797, -165.2084106276440423, 41.63779006702063867 ) ) ;
#1534 = CARTESIAN_POINT ( 'NONE',  ( -143.8425227516148084, -186.6938272943107222, 55.19815736654470584 ) ) ;
#1536 = FACE_OUTER_BOUND ( 'NONE', #21519, .T. ) ;
#1535 = CARTESIAN_POINT ( 'NONE',  ( -120.0322075325610740, -126.9891397928655010, 49.65701158161630957 ) ) ;
#1537 = CARTESIAN_POINT ( 'NONE',  ( 165.8083469658213005, 192.9029763258799335, -44.99999999999997158 ) ) ;
#1538 = ADVANCED_FACE ( 'NONE', ( #15287 ), #10546, .F. ) ;
#1539 = CARTESIAN_POINT ( 'NONE',  ( 41.46631938032478359, 147.1104996726487570, 29.45539723777780239 ) ) ;
#1540 = CARTESIAN_POINT ( 'NONE',  ( 48.01140435219951996, 115.1344580088725991, 35.83527830041809636 ) ) ;
#1541 = CARTESIAN_POINT ( 'NONE',  ( 45.74753988029933538, 64.16518717409400097, 37.97664729208901946 ) ) ;
#1542 = CARTESIAN_POINT ( 'NONE',  ( -151.4692556286852891, -126.9891397928655010, -64.65701158161634510 ) ) ;
#1543 = EDGE_CURVE ( 'NONE', #18069, #12813, #20253, .T. ) ;
#1544 = CARTESIAN_POINT ( 'NONE',  ( 47.30009524607925897, 85.94413156685014599, 0.1962900075584997628 ) ) ;
#1545 = CARTESIAN_POINT ( 'NONE',  ( 45.74753988029934249, 148.1651871740940010, 37.97664729208901235 ) ) ;
#1546 = CARTESIAN_POINT ( 'NONE',  ( -154.3824083646099439, -157.2938272943107449, 58.62277379824867296 ) ) ;
#1547 = CARTESIAN_POINT ( 'NONE',  ( -151.4692556286852891, -179.9084106276440593, 39.74470866294723947 ) ) ;
#1548 = ORIENTED_EDGE ( 'NONE', *, *, #12026, .F. ) ;
#1549 = CARTESIAN_POINT ( 'NONE',  ( 43.01140435219951286, 78.53445800887259054, 39.21067981925356349 ) ) ;
#1550 = CARTESIAN_POINT ( 'NONE',  ( -148.5561028927606344, -157.2584106276440536, 58.62277379824867296 ) ) ;
#1551 = CARTESIAN_POINT ( 'NONE',  ( 22.89857099655110062, 139.5608133708311982, -4.966967973427480310 ) ) ;
#1552 = CARTESIAN_POINT ( 'NONE',  ( -158.9748091281504401, -126.9891397928655010, 36.65701158161628115 ) ) ;
#1553 = CARTESIAN_POINT ( 'NONE',  ( 45.74753988029933538, 128.0651871740940067, 30.44471234641811819 ) ) ;
#1554 = CARTESIAN_POINT ( 'NONE',  ( 17.52322149637394233, 97.17389352242535949, -4.727774211004094340 ) ) ;
#1555 = VERTEX_POINT ( 'NONE', #12182 ) ;
#1556 = ORIENTED_EDGE ( 'NONE', *, *, #9958, .F. ) ;
#1557 = DIRECTION ( 'NONE',  ( -0.3450121214752279175, 0.9385982292947087080, 0.000000000000000000 ) ) ;
#1558 = ORIENTED_EDGE ( 'NONE', *, *, #4729, .F. ) ;
#1559 = CARTESIAN_POINT ( 'NONE',  ( 38.96631938032478359, 108.0844580088725877, 37.14960608071593384 ) ) ;
#1560 = CARTESIAN_POINT ( 'NONE',  ( 44.37947211624943833, 155.4797705074273324, 30.00020018409699318 ) ) ;
#1561 = EDGE_CURVE ( 'NONE', #6540, #20418, #2056, .T. ) ;
#1562 = CARTESIAN_POINT ( 'NONE',  ( 41.64333658814960870, 68.77977050742731535, 30.00020018409699318 ) ) ;
#1564 = CARTESIAN_POINT ( 'NONE',  ( 25.21830160582964453, 141.7844325674071229, 10.15653385063274428 ) ) ;
#1563 = CARTESIAN_POINT ( 'NONE',  ( 40.27526882409969033, 123.5651871740939924, 37.97664729208901946 ) ) ;
#1565 = CIRCLE ( 'NONE', #17047, 7.500000000000007105 ) ;
#1566 = CARTESIAN_POINT ( 'NONE',  ( 39.92123440845004723, 78.26049967264873430, 29.95742577749337343 ) ) ;
#1567 = CARTESIAN_POINT ( 'NONE',  ( 15.97061701817242785, 140.8453463817331794, 16.82122940411608170 ) ) ;
#1568 = CARTESIAN_POINT ( 'NONE',  ( 42.21948215057684450, 144.0373810949689641, 29.21067981925356705 ) ) ;
#1569 = DIRECTION ( 'NONE',  ( -1.000000000000000000, 0.000000000000000000, 0.000000000000000000 ) ) ;
#1570 = CARTESIAN_POINT ( 'NONE',  ( 44.37947211624943833, 88.01518717409399528, 38.42115945441014446 ) ) ;
#1571 = CARTESIAN_POINT ( 'NONE',  ( 39.92123440845005433, 81.26049967264872009, 29.95742577749336988 ) ) ;
#1572 = DIRECTION ( 'NONE',  ( -1.000000000000000000, 0.000000000000000000, 0.000000000000000000 ) ) ;
#1573 = VERTEX_POINT ( 'NONE', #18482 ) ;
#1574 = CARTESIAN_POINT ( 'NONE',  ( 46.59305225739526435, 64.57977050742731251, 36.81289934271958941 ) ) ;
#1575 = CARTESIAN_POINT ( 'NONE',  ( -151.4692556286852891, -187.4084106276440309, 59.56931450028537967 ) ) ;
#1576 = CARTESIAN_POINT ( 'NONE',  ( 53.71239221804358976, 87.38980250447106357, 6.982120393166105998 ) ) ;
#1577 = CARTESIAN_POINT ( 'NONE',  ( -154.3824083646099439, -185.7584106276440536, 40.69124936498395328 ) ) ;
#1578 = ORIENTED_EDGE ( 'NONE', *, *, #8963, .T. ) ;
#1579 = CARTESIAN_POINT ( 'NONE',  ( 44.37947211624943833, 149.2151871740940123, 30.00020018409699318 ) ) ;
#1580 = DIRECTION ( 'NONE',  ( -0.000000000000000000, 0.000000000000000000, -1.000000000000000000 ) ) ;
#1581 = AXIS2_PLACEMENT_3D ( 'NONE', #1237, #19759, #16328 ) ;
#1582 = CARTESIAN_POINT ( 'NONE',  ( 47.43856463449118621, 112.8797705074273097, 34.21067981925357060 ) ) ;
#1583 = CARTESIAN_POINT ( 'NONE',  ( 40.73010619540765020, 85.74955863377461185, -6.589596535617429751 ) ) ;
#1584 = VERTEX_POINT ( 'NONE', #10112 ) ;
#1585 = CARTESIAN_POINT ( 'NONE',  ( 26.70363248220801466, 142.8423586596025245, -10.77201286955609127 ) ) ;
#1586 = ORIENTED_EDGE ( 'NONE', *, *, #14863, .T. ) ;
#1587 = CARTESIAN_POINT ( 'NONE',  ( 24.43941541943582862, 313.3049502139530205, -19.99999999999997868 ) ) ;
#1588 = CARTESIAN_POINT ( 'NONE',  ( 41.64333658814960870, 150.7151871740940123, 38.42115945441014446 ) ) ;
#1589 = CARTESIAN_POINT ( 'NONE',  ( 62.62098228421420032, 91.94359626243755201, 7.653270806628301948 ) ) ;
#1590 = PLANE ( 'NONE',  #20674 ) ;
#1591 = DIRECTION ( 'NONE',  ( -1.000000000000000000, 0.000000000000000000, -0.000000000000000000 ) ) ;
#1592 = CARTESIAN_POINT ( 'NONE',  ( 43.01140435219951996, 10.71049967264875491, 34.21067981925357060 ) ) ;
#1593 = CARTESIAN_POINT ( 'NONE',  ( -161.4692556286853176, -176.4891397928654442, 49.65701158161630957 ) ) ;
#1594 = CARTESIAN_POINT ( 'NONE',  ( 43.01140435219951996, 10.71049967264875491, 39.21067981925356349 ) ) ;
#1595 = CARTESIAN_POINT ( 'NONE',  ( -157.6495955161842062, -194.9391397928654897, 41.15050349809589392 ) ) ;
#1596 = CARTESIAN_POINT ( 'NONE',  ( 38.58424406990784661, 96.22977050742728977, 32.77220824515698183 ) ) ;
#1597 = CARTESIAN_POINT ( 'NONE',  ( 57.03263806925237844, 95.34629841206742640, 19.84245794357962822 ) ) ;
#1598 = CARTESIAN_POINT ( 'NONE',  ( -159.0959885057557983, -184.5938272943107279, 55.19815736654470584 ) ) ;
#1599 = CARTESIAN_POINT ( 'NONE',  ( 39.42975644700377558, 90.41518717409400097, 36.81289934271958941 ) ) ;
#1600 = CARTESIAN_POINT ( 'NONE',  ( 38.01140435219952707, 84.56049967264873146, 32.58608133808903773 ) ) ;
#1601 = AXIS2_PLACEMENT_3D ( 'NONE', #19582, #1512, #8350 ) ;
#1602 = ORIENTED_EDGE ( 'NONE', *, *, #13466, .F. ) ;
#1603 = CYLINDRICAL_SURFACE ( 'NONE', #18577, 4.999999999999997335 ) ;
#1604 = CARTESIAN_POINT ( 'NONE',  ( 76.40658810299491677, 127.4365358892444959, 12.33923360994393903 ) ) ;
#1605 = CARTESIAN_POINT ( 'NONE',  ( 54.97053026609068382, 94.45704024927961484, -6.077358488390353308 ) ) ;
#1606 = CARTESIAN_POINT ( 'NONE',  ( 47.43856463449117911, 61.72977050742730398, 35.64915139335015937 ) ) ;
#1607 =( BOUNDED_CURVE ( )  B_SPLINE_CURVE ( 2, ( #12617, #17569, #17677, #610, #9317, #19023, #16019, #7676, #12285, #824, #9216, #7560, #14258 ),
 .UNSPECIFIED., .F., .F. ) 
 B_SPLINE_CURVE_WITH_KNOTS ( ( 3, 2, 2, 2, 2, 2, 3 ),
 ( 0.2867647058823529216, 0.2882352941176470340, 0.2911764705882353144, 0.2941176470588235392, 0.2970588235294117641, 0.2999999999999999889, 0.3014705882352941013 ),
 .UNSPECIFIED. ) 
 CURVE ( )  GEOMETRIC_REPRESENTATION_ITEM ( )  RATIONAL_B_SPLINE_CURVE ( ( 0.9755282581475768211, 0.9755282581475768211, 1.000000000000000000, 0.9510565162951535312, 1.000000000000000000, 0.9510565162951535312, 1.000000000000000000, 0.9510565162951535312, 1.000000000000000000, 0.9510565162951535312, 1.000000000000000000, 0.9755282581475768211, 0.9755282581475768211 ) ) 
 REPRESENTATION_ITEM ( '' )  );
#1608 = VERTEX_POINT ( 'NONE', #16926 ) ;
#1609 = CARTESIAN_POINT ( 'NONE',  ( 38.58424406990784661, 144.5297705074273154, 35.64915139335016647 ) ) ;
#1610 = EDGE_CURVE ( 'NONE', #1195, #15871, #4962, .T. ) ;
#1611 = CARTESIAN_POINT ( 'NONE',  ( 44.37947211624943833, 97.27977050742732956, 38.42115945441014446 ) ) ;
#1612 = CYLINDRICAL_SURFACE ( 'NONE', #21460, 7.500000000000007105 ) ;
#1613 = AXIS2_PLACEMENT_3D ( 'NONE', #14650, #9274, #21390 ) ;
#1614 = CARTESIAN_POINT ( 'NONE',  ( 44.55648932407425633, 110.8104996726487457, 29.45539723777780239 ) ) ;
#1615 = CARTESIAN_POINT ( 'NONE',  ( 38.58424406990784661, 71.96518717409399812, 32.77220824515698183 ) ) ;
#1616 = DIRECTION ( 'NONE',  ( 0.000000000000000000, 0.000000000000000000, -1.000000000000000000 ) ) ;
#1617 = CARTESIAN_POINT ( 'NONE',  ( -143.8425227516148084, -165.6938272943107222, 55.19815736654470584 ) ) ;
#1618 = DIRECTION ( 'NONE',  ( -0.000000000000000000, 1.000000000000000000, -0.000000000000000000 ) ) ;
#1619 = CARTESIAN_POINT ( 'NONE',  ( -161.4692556286852607, -178.4130981290893203, 52.90620854394536821 ) ) ;
#1620 = CARTESIAN_POINT ( 'NONE',  ( 39.92123440845005433, 112.1604996726487258, 38.46393386101375711 ) ) ;
#1621 = CARTESIAN_POINT ( 'NONE',  ( 43.01140435219951286, 150.5344580088725479, 39.46799094044489209 ) ) ;
#1622 = CARTESIAN_POINT ( 'NONE',  ( 39.42975644700377558, 126.6797705074273210, 36.81289934271958941 ) ) ;
#1623 = CARTESIAN_POINT ( 'NONE',  ( 63.63589212299756070, 92.48244826560708987, 12.62055557379543203 ) ) ;
#1624 = CARTESIAN_POINT ( 'NONE',  ( 48.01140435219951996, 95.21049967264875136, 34.21067981925357060 ) ) ;
#1625 = CARTESIAN_POINT ( 'NONE',  ( 47.43856463449117911, 112.4651871740939981, 35.64915139335015937 ) ) ;
#1626 = CARTESIAN_POINT ( 'NONE',  ( -159.5594255724347761, -167.1891397928654897, 55.53486410454104316 ) ) ;
#1627 = CYLINDRICAL_SURFACE ( 'NONE', #21761, 4.999999999999997335 ) ;
#1628 = CARTESIAN_POINT ( 'NONE',  ( 67.48508721674359379, 143.7297851702464015, -1.275552590249036777 ) ) ;
#1629 = CARTESIAN_POINT ( 'NONE',  ( 49.55020742284296631, 92.47612394764220767, 0.1565338505643876776 ) ) ;
#1630 = VECTOR ( 'NONE', #21496, 1000.000000000000000 ) ;
#1631 = DIRECTION ( 'NONE',  ( 0.000000000000000000, -1.000000000000000000, 0.000000000000000000 ) ) ;
#1632 = CARTESIAN_POINT ( 'NONE',  ( 44.37947211624943833, 97.27977050742732956, 38.42115945441014446 ) ) ;
#1633 = CIRCLE ( 'NONE', #16042, 9.999999999999994671 ) ;
#1634 = EDGE_LOOP ( 'NONE', ( #6697, #6090, #8259, #12227, #10323, #12958 ) ) ;
#1635 = DIRECTION ( 'NONE',  ( 1.000000000000000000, 0.000000000000000000, 0.000000000000000000 ) ) ;
#1636 = EDGE_LOOP ( 'NONE', ( #13666, #2702 ) ) ;
#1637 = CARTESIAN_POINT ( 'NONE',  ( 43.01140435219951286, 71.03445800887256212, 28.95336869806222779 ) ) ;
#1638 = DIRECTION ( 'NONE',  ( -0.000000000000000000, -0.000000000000000000, 1.000000000000000000 ) ) ;
#1639 = CARTESIAN_POINT ( 'NONE',  ( 44.55648932407425633, 140.8104996726487457, 29.45539723777780239 ) ) ;
#1641 = CARTESIAN_POINT ( 'NONE',  ( 54.44380493464903736, 94.21656919670213881, 0.9465279732350617703 ) ) ;
#1640 = CARTESIAN_POINT ( 'NONE',  ( 46.59305225739526435, 94.91518717409400097, 31.60846029578754468 ) ) ;
#1642 = ADVANCED_FACE ( 'NONE', ( #8572 ), #13730, .F. ) ;
#1643 = CIRCLE ( 'NONE', #19950, 5.000000000000004441 ) ;
#1644 = CARTESIAN_POINT ( 'NONE',  ( -148.5561028927606344, -168.0584106276440366, 40.69124936498395328 ) ) ;
#1645 = CARTESIAN_POINT ( 'NONE',  ( -154.3824083646099439, -191.4938272943107336, 40.69124936498395328 ) ) ;
#1647 = CARTESIAN_POINT ( 'NONE',  ( 47.05648932407426344, 69.98445800887257917, 37.14960608071593384 ) ) ;
#1646 = LINE ( 'NONE', #11664, #7653 ) ;
#1648 = CARTESIAN_POINT ( 'NONE',  ( -141.4692556286852891, -189.0630981290892976, 49.65701158161630957 ) ) ;
#1649 = ADVANCED_BREP_SHAPE_REPRESENTATION ( '', ( #7211, #12657 ), #7417 ) ;
#1650 = CARTESIAN_POINT ( 'NONE',  ( -143.3790856849358306, -176.7630981290893146, 43.77915905869157598 ) ) ;
#1651 = CARTESIAN_POINT ( 'NONE',  ( 42.21948215057684450, 78.03738109496902098, 29.21067981925356705 ) ) ;
#1652 = CARTESIAN_POINT ( 'NONE',  ( 44.37947211624943833, 148.2797705074273154, 38.42115945441014446 ) ) ;
#1653 = CARTESIAN_POINT ( 'NONE',  ( 73.72238702602700755, 135.0318370961144296, 5.077453337991364002 ) ) ;
#1654 = CARTESIAN_POINT ( 'NONE',  ( 39.42975644700377558, 140.8151871740940067, 31.60846029578754468 ) ) ;
#1655 = CARTESIAN_POINT ( 'NONE',  ( -143.8425227516148084, -162.6938272943107222, 55.19815736654470584 ) ) ;
#1656 = CARTESIAN_POINT ( 'NONE',  ( -145.6429501568359797, -175.1084106276440480, 57.67623309621197336 ) ) ;
#1657 = ORIENTED_EDGE ( 'NONE', *, *, #8443, .F. ) ;
#1658 = CARTESIAN_POINT ( 'NONE',  ( -157.2955611005346270, -158.6084106276440480, 41.63779006702063867 ) ) ;
#1659 = CARTESIAN_POINT ( 'NONE',  ( 66.44170838958859804, 135.7440291252205213, 4.009006963233090026 ) ) ;
#1660 = LINE ( 'NONE', #8607, #8486 ) ;
#1661 = CARTESIAN_POINT ( 'NONE',  ( 40.27526882409969033, 120.5651871740940209, 37.97664729208901946 ) ) ;
#1662 = EDGE_CURVE ( 'NONE', #9722, #11465, #14251, .T. ) ;
#1663 = VECTOR ( 'NONE', #13216, 1000.000000000000114 ) ;
#1664 = VERTEX_POINT ( 'NONE', #16023 ) ;
#1665 = EDGE_LOOP ( 'NONE', ( #5611, #19532, #4554, #12412 ) ) ;
#1666 = CARTESIAN_POINT ( 'NONE',  ( 38.96631938032478359, 146.4844580088725934, 31.27175355779120025 ) ) ;
#1667 = ORIENTED_EDGE ( 'NONE', *, *, #1675, .T. ) ;
#1668 = EDGE_CURVE ( 'NONE', #4967, #19403, #16139, .T. ) ;
#1669 = CARTESIAN_POINT ( 'NONE',  ( 38.01140435219952707, 107.7844580088725763, 34.21067981925357060 ) ) ;
#1670 = CARTESIAN_POINT ( 'NONE',  ( 45.74753988029934249, 154.4297705074272926, 37.97664729208901235 ) ) ;
#1671 = CARTESIAN_POINT ( 'NONE',  ( 46.59305225739526435, 64.57977050742731251, 36.81289934271958941 ) ) ;
#1673 = CARTESIAN_POINT ( 'NONE',  ( 70.94289844336020678, 123.7826807253454575, 5.513563639855703080 ) ) ;
#1672 = CARTESIAN_POINT ( 'NONE',  ( 43.01140435219951286, 125.3651871740940180, 29.55568802177586463 ) ) ;
#1674 =( BOUNDED_CURVE ( )  B_SPLINE_CURVE ( 2, ( #298, #17145, #8790, #12624, #20789, #14165, #17980, #19346, #617, #5894, #7972, #3001, #5681 ),
 .UNSPECIFIED., .F., .F. ) 
 B_SPLINE_CURVE_WITH_KNOTS ( ( 3, 2, 2, 2, 2, 2, 3 ),
 ( 0.4779411764705882582, 0.4794117647058823706, 0.4823529411764705954, 0.4852941176470588203, 0.4882352941176470451, 0.4911764705882352700, 0.4926470588235293824 ),
 .UNSPECIFIED. ) 
 CURVE ( )  GEOMETRIC_REPRESENTATION_ITEM ( )  RATIONAL_B_SPLINE_CURVE ( ( 0.9755282581475768211, 0.9755282581475772652, 1.000000000000000000, 0.9510565162951535312, 1.000000000000000000, 0.9510565162951535312, 1.000000000000000000, 0.9510565162951535312, 1.000000000000000000, 0.9510565162951535312, 1.000000000000000000, 0.9755282581475772652, 0.9755282581475768211 ) ) 
 REPRESENTATION_ITEM ( '' )  );
#1675 = EDGE_CURVE ( 'NONE', #16415, #5871, #2693, .T. ) ;
#1676 = VECTOR ( 'NONE', #18323, 1000.000000000000000 ) ;
#1677 = CARTESIAN_POINT ( 'NONE',  ( 44.55648932407425633, 86.81049967264874567, 29.45539723777780239 ) ) ;
#1678 = DIRECTION ( 'NONE',  ( -0.000000000000000000, 1.000000000000000000, -0.000000000000000000 ) ) ;
#1679 = CARTESIAN_POINT ( 'NONE',  ( 47.05648932407426344, 98.51049967264874851, 31.27175355779120025 ) ) ;
#1680 = CARTESIAN_POINT ( 'NONE',  ( 18.67254549292281141, -61.68114226949890622, 30.00000000000000000 ) ) ;
#1681 = CARTESIAN_POINT ( 'NONE',  ( 47.43856463449118621, 85.61518717409400381, 34.21067981925357060 ) ) ;
#1682 = AXIS2_PLACEMENT_3D ( 'NONE', #6827, #13534, #14958 ) ;
#1683 = CARTESIAN_POINT ( 'NONE',  ( 43.01140435219951286, 72.53445800887256212, 39.21067981925356349 ) ) ;
#1684 = VERTEX_POINT ( 'NONE', #20895 ) ;
#1685 = CARTESIAN_POINT ( 'NONE',  ( 47.43856463449117200, 61.72977050742730398, 35.64915139335016647 ) ) ;
#1686 = CARTESIAN_POINT ( 'NONE',  ( -154.3824083646099439, -185.7584106276440536, 40.69124936498395328 ) ) ;
#1687 = CARTESIAN_POINT ( 'NONE',  ( 75.87089013534350102, 129.7906142932847331, -2.736556584054479657 ) ) ;
#1688 = CARTESIAN_POINT ( 'NONE',  ( -145.6429501568359797, -175.1084106276440480, 57.67623309621198047 ) ) ;
#1689 = ORIENTED_EDGE ( 'NONE', *, *, #18515, .T. ) ;
#1690 = EDGE_CURVE ( 'NONE', #12769, #10070, #4754, .T. ) ;
#1691 = CARTESIAN_POINT ( 'NONE',  ( 41.64333658814960870, 150.7151871740940123, 38.42115945441014446 ) ) ;
#1692 = CARTESIAN_POINT ( 'NONE',  ( -39.63192160874135084, -37.13255853780189852, 20.00000000000002132 ) ) ;
#1693 = CARTESIAN_POINT ( 'NONE',  ( 39.42975644700377558, 111.0797705074273125, 31.60846029578754468 ) ) ;
#1694 = CARTESIAN_POINT ( 'NONE',  ( 69.71972837475884432, 98.49221204361529658, -7.660766391518695428 ) ) ;
#1695 = VECTOR ( 'NONE', #20159, 1000.000000000000000 ) ;
#1696 = VERTEX_POINT ( 'NONE', #5891 ) ;
#1697 = EDGE_CURVE ( 'NONE', #15900, #2204, #8782, .T. ) ;
#1698 = CARTESIAN_POINT ( 'NONE',  ( 16.33471683235446292, 110.7640000046674089, -5.200637885961103102 ) ) ;
#1699 = VERTEX_POINT ( 'NONE', #2375 ) ;
#1700 = CARTESIAN_POINT ( 'NONE',  ( 47.43856463449118621, 121.8797705074273239, 34.21067981925357060 ) ) ;
#1701 = PRESENTATION_LAYER_ASSIGNMENT (  '', '', ( #6635 ) ) ;
#1702 = DIRECTION ( 'NONE',  ( 0.000000000000000000, -1.000000000000000000, 0.000000000000000000 ) ) ;
#1703 = CARTESIAN_POINT ( 'NONE',  ( 43.01140435219951286, 153.8651871740939612, 38.86567161673127657 ) ) ;
#1704 = CARTESIAN_POINT ( 'NONE',  ( 71.86557814238962294, 101.4853659568252766, -7.779689512009451136 ) ) ;
#1705 = CARTESIAN_POINT ( 'NONE',  ( 47.05648932407426344, 81.98445800887257917, 37.14960608071593384 ) ) ;
#1706 = CARTESIAN_POINT ( 'NONE',  ( -157.6495955161842062, -182.9391397928654612, 41.15050349809590102 ) ) ;
#1707 = DIRECTION ( 'NONE',  ( 0.000000000000000000, -1.000000000000000000, 0.000000000000000000 ) ) ;
#1708 = DIRECTION ( 'NONE',  ( 0.000000000000000000, 1.000000000000000000, 0.000000000000000000 ) ) ;
#1709 = CARTESIAN_POINT ( 'NONE',  ( -151.4692556286852891, -136.9891397928655010, 39.65701158161630246 ) ) ;
#1710 = CARTESIAN_POINT ( 'NONE',  ( 39.92123440845005433, 98.33445800887258770, 29.95742577749336988 ) ) ;
#1711 = CARTESIAN_POINT ( 'NONE',  ( 40.27526882409969033, 90.82977050742731251, 37.97664729208901946 ) ) ;
#1712 = CARTESIAN_POINT ( 'NONE',  ( 71.19430100617981338, 118.9508470517051535, -8.295922056425867552 ) ) ;
#1713 = CARTESIAN_POINT ( 'NONE',  ( -151.4692556286852891, -170.6438272943107677, 39.74470866294723947 ) ) ;
#1714 = CARTESIAN_POINT ( 'NONE',  ( 40.27526882409969744, 87.56518717409400665, 37.97664729208901235 ) ) ;
#1715 = CARTESIAN_POINT ( 'NONE',  ( 0.08333186253067781379, 634.6318465664365931, -3.999999999999996447 ) ) ;
#1716 = ORIENTED_EDGE ( 'NONE', *, *, #20163, .F. ) ;
#1717 = EDGE_CURVE ( 'NONE', #16694, #21813, #4400, .T. ) ;
#1718 = EDGE_CURVE ( 'NONE', #7475, #15486, #20604, .T. ) ;
#1719 = CARTESIAN_POINT ( 'NONE',  ( 38.96631938032478359, 137.4844580088725650, 31.27175355779120025 ) ) ;
#1720 = SHAPE_REPRESENTATION ( 'Blade Pivot Hinge Pin', ( #12657 ), #4220 ) ;
#1721 = CARTESIAN_POINT ( 'NONE',  ( 9.231363607564425422, 125.4582397780895633, 16.26765482522027639 ) ) ;
#1722 = CARTESIAN_POINT ( 'NONE',  ( 43.01140435219951286, 142.1297705074273097, 38.86567161673127657 ) ) ;
#1723 = CARTESIAN_POINT ( 'NONE',  ( 24.98902006629997175, 141.4916631675600343, -2.862956674147950409 ) ) ;
#1724 = FACE_OUTER_BOUND ( 'NONE', #3351, .T. ) ;
#1725 = ORIENTED_EDGE ( 'NONE', *, *, #10803, .F. ) ;
#1726 = CARTESIAN_POINT ( 'NONE',  ( 47.43856463449118621, 145.8797705074273097, 34.21067981925357060 ) ) ;
#1727 = CARTESIAN_POINT ( 'NONE',  ( 41.64333658814960870, 95.77977050742732956, 30.00020018409699318 ) ) ;
#1728 = FACE_OUTER_BOUND ( 'NONE', #336, .T. ) ;
#1729 = CARTESIAN_POINT ( 'NONE',  ( 173.3794444120442506, -126.9891397928655010, 67.64809332337412684 ) ) ;
#1730 = CARTESIAN_POINT ( 'NONE',  ( -153.0531000319306827, -170.2362167067689995, 39.65701158161629536 ) ) ;
#1731 = CARTESIAN_POINT ( 'NONE',  ( -159.0959885057557983, -164.1938272943107222, 44.11586579668791330 ) ) ;
#1732 = CARTESIAN_POINT ( 'NONE',  ( -159.5594255724347761, -169.2630981290892862, 55.53486410454104316 ) ) ;
#1733 = CARTESIAN_POINT ( 'NONE',  ( 38.01140435219952707, 111.7104996726487514, 34.21067981925357060 ) ) ;
#1734 = CARTESIAN_POINT ( 'NONE',  ( 43.01140435219951286, 146.0344580088725195, 28.95336869806222779 ) ) ;
#1735 = CARTESIAN_POINT ( 'NONE',  ( 41.64333658814960870, 122.7797705074273296, 30.00020018409699318 ) ) ;
#1736 = CARTESIAN_POINT ( 'NONE',  ( 71.19881468907274780, 122.2058620619881566, -2.419290889312981641 ) ) ;
#1737 = CARTESIAN_POINT ( 'NONE',  ( 38.01140435219952707, 140.7844580088725763, 34.21067981925357060 ) ) ;
#1738 = CARTESIAN_POINT ( 'NONE',  ( 46.59305225739526435, 121.3151871740940067, 36.81289934271958941 ) ) ;
#1739 = ADVANCED_FACE ( 'NONE', ( #20787 ), #16724, .T. ) ;
#1740 = DIRECTION ( 'NONE',  ( 0.000000000000000000, 0.000000000000000000, 1.000000000000000000 ) ) ;
#1741 = DIRECTION ( 'NONE',  ( -0.000000000000000000, -0.000000000000000000, 1.000000000000000000 ) ) ;
#1742 = CARTESIAN_POINT ( 'NONE',  ( 42.70556344282044137, 85.75549003223034106, 1.343541076088082376 ) ) ;
#1743 = CARTESIAN_POINT ( 'NONE',  ( 62.66823040046688931, 140.1266048904901993, -2.224326160187301227 ) ) ;
#1744 = CARTESIAN_POINT ( 'NONE',  ( -104.7439762501682736, 39.86119447055682485, 4.000000000000021316 ) ) ;
#1745 = AXIS2_PLACEMENT_3D ( 'NONE', #8370, #15081, #21817 ) ;
#1746 = CARTESIAN_POINT ( 'NONE',  ( 47.43856463449117911, 82.72977050742731819, 35.64915139335015937 ) ) ;
#1747 = EDGE_CURVE ( 'NONE', #4207, #19742, #20682, .T. ) ;
#1748 = ORIENTED_EDGE ( 'NONE', *, *, #3444, .T. ) ;
#1749 = CARTESIAN_POINT ( 'NONE',  ( -143.3790856849358306, -168.3630981290893089, 55.53486410454105027 ) ) ;
#1750 = CARTESIAN_POINT ( 'NONE',  ( 38.01140435219951996, 71.93445800887258201, 35.83527830041810347 ) ) ;
#1751 = DIRECTION ( 'NONE',  ( 0.000000000000000000, 0.000000000000000000, 1.000000000000000000 ) ) ;
#1752 = CARTESIAN_POINT ( 'NONE',  ( 46.10157429594899270, 139.7604996726487627, 38.46393386101376421 ) ) ;
#1754 = CARTESIAN_POINT ( 'NONE',  ( 29.68407903333335085, 144.6596297928226988, 11.33750686376150085 ) ) ;
#1753 = CARTESIAN_POINT ( 'NONE',  ( 43.01140435219951286, 90.86518717409400381, 38.86567161673127657 ) ) ;
#1755 = CARTESIAN_POINT ( 'NONE',  ( -143.8425227516148084, -156.3584106276440480, 44.11586579668791330 ) ) ;
#1756 = CARTESIAN_POINT ( 'NONE',  ( -142.0420953463935803, -189.2438272943107052, 46.59394152635518083 ) ) ;
#1757 = CARTESIAN_POINT ( 'NONE',  ( 38.96631938032478359, 93.41049967264873999, 31.27175355779120025 ) ) ;
#1758 = CARTESIAN_POINT ( 'NONE',  ( 43.01140435219951286, 128.0344580088725479, 29.21067981925356705 ) ) ;
#1759 = CARTESIAN_POINT ( 'NONE',  ( 38.96631938032478359, 148.0104996726487627, 37.14960608071593384 ) ) ;
#1760 = CARTESIAN_POINT ( 'NONE',  ( -176.9699209214867608, -136.9891397928655010, -35.00000000000000000 ) ) ;
#1761 = CARTESIAN_POINT ( 'NONE',  ( 38.58424406990784661, 156.5297705074272869, 35.64915139335016647 ) ) ;
#1762 = CARTESIAN_POINT ( 'NONE',  ( 151.4773229304660731, 84.89323405393692212, 14.00000000000001776 ) ) ;
#1763 = CARTESIAN_POINT ( 'NONE',  ( 9.468627745026951814, 113.0646104733145592, 1.862908727141013854 ) ) ;
#1764 = CARTESIAN_POINT ( 'NONE',  ( 46.59305225739526435, 145.3151871740940067, 36.81289934271958941 ) ) ;
#1765 = CARTESIAN_POINT ( 'NONE',  ( -151.4692556286852891, -158.6438272943107108, 39.74470866294723947 ) ) ;
#1766 = CARTESIAN_POINT ( 'NONE',  ( -142.0420953463936087, -174.6584106276440593, 49.65701158161630957 ) ) ;
#1767 = ORIENTED_EDGE ( 'NONE', *, *, #7862, .T. ) ;
#1768 = DIRECTION ( 'NONE',  ( 1.000000000000000000, 0.000000000000000000, 5.966140889015784385E-16 ) ) ;
#1769 = CARTESIAN_POINT ( 'NONE',  ( -154.3824083646099439, -164.7584106276440536, 40.69124936498395328 ) ) ;
#1770 = CARTESIAN_POINT ( 'NONE',  ( 18.91286941000743838, 105.1068529970173699, 0.5568269029779387980 ) ) ;
#1771 = CARTESIAN_POINT ( 'NONE',  ( 39.92123440845005433, 134.3344580088725877, 29.95742577749336988 ) ) ;
#1772 = CARTESIAN_POINT ( 'NONE',  ( 38.58424406990784661, 128.9651871740939839, 32.77220824515698183 ) ) ;
#1773 = EDGE_CURVE ( 'NONE', #11679, #1573, #7680, .T. ) ;
#1774 = ORIENTED_EDGE ( 'NONE', *, *, #5185, .T. ) ;
#1775 = ORIENTED_EDGE ( 'NONE', *, *, #1391, .T. ) ;
#1776 =( GEOMETRIC_REPRESENTATION_CONTEXT ( 3 ) GLOBAL_UNCERTAINTY_ASSIGNED_CONTEXT ( ( #14131 ) ) GLOBAL_UNIT_ASSIGNED_CONTEXT ( ( #2724, #2506, #19371 ) ) REPRESENTATION_CONTEXT ( 'NONE', 'WORKASPACE' ) );
#1777 = CARTESIAN_POINT ( 'NONE',  ( 41.46631938032478359, 114.3844580088725849, 38.96596240072933170 ) ) ;
#1778 = ORIENTED_EDGE ( 'NONE', *, *, #3369, .T. ) ;
#1779 = CARTESIAN_POINT ( 'NONE',  ( 41.46631938032478359, 98.18445800887256780, 29.45539723777780239 ) ) ;
#1780 = CARTESIAN_POINT ( 'NONE',  ( 39.42975644700377558, 156.0797705074273267, 31.60846029578754468 ) ) ;
#1781 = CARTESIAN_POINT ( 'NONE',  ( 43.01140435219951286, 67.12977050742732388, 38.86567161673127657 ) ) ;
#1783 = CARTESIAN_POINT ( 'NONE',  ( 53.64127281404707048, 146.0262708631457542, 11.34682183016344403 ) ) ;
#1782 = CARTESIAN_POINT ( 'NONE',  ( 44.37947211624943833, 127.0151871740939953, 38.42115945441014446 ) ) ;
#1784 = EDGE_CURVE ( 'NONE', #10393, #12279, #9220, .T. ) ;
#1785 = CARTESIAN_POINT ( 'NONE',  ( 46.10157429594899270, 85.76049967264873430, 38.46393386101376421 ) ) ;
#1786 = DIRECTION ( 'NONE',  ( -0.000000000000000000, -0.000000000000000000, -1.000000000000000000 ) ) ;
#1787 = DIRECTION ( 'NONE',  ( 0.3450121214752279175, -0.9385982292947087080, -0.000000000000000000 ) ) ;
#1788 = CARTESIAN_POINT ( 'NONE',  ( -27.64582385433943656, -34.13255853780189142, 5.000000000000018652 ) ) ;
#1789 = ADVANCED_FACE ( 'NONE', ( #14377 ), #15918, .T. ) ;
#1790 = CARTESIAN_POINT ( 'NONE',  ( 44.37947211624943833, 80.21518717409399812, 30.00020018409699318 ) ) ;
#1791 = PRODUCT_DEFINITION_CONTEXT ( 'detailed design', #289, 'design' ) ;
#1792 = CARTESIAN_POINT ( 'NONE',  ( 39.03606557573836255, 144.5896687849443651, 31.16068397573688387 ) ) ;
#1793 = DIRECTION ( 'NONE',  ( 0.000000000000000000, 0.000000000000000000, 1.000000000000000000 ) ) ;
#1794 = AXIS2_PLACEMENT_3D ( 'NONE', #761, #5605, #2201 ) ;
#1795 = ORIENTED_EDGE ( 'NONE', *, *, #13768, .T. ) ;
#1796 = CARTESIAN_POINT ( 'NONE',  ( 39.42975644700377558, 66.67977050742732104, 36.81289934271958941 ) ) ;
#1797 = CARTESIAN_POINT ( 'NONE',  ( -160.8964159109769696, -191.3084106276440650, 46.59394152635518793 ) ) ;
#1798 = CARTESIAN_POINT ( 'NONE',  ( 64.81014823317600815, 93.40725510594978687, -1.427111354441281899 ) ) ;
#1799 = CARTESIAN_POINT ( 'NONE',  ( -151.4692556286852891, -173.9084106276440593, 39.74470866294723947 ) ) ;
#1800 = VERTEX_POINT ( 'NONE', #17680 ) ;
#1801 = CARTESIAN_POINT ( 'NONE',  ( 44.37947211624943833, 157.0151871740940237, 38.42115945441014446 ) ) ;
#1802 = CARTESIAN_POINT ( 'NONE',  ( 43.01140435219951286, 116.6297705074273097, 29.55568802177586107 ) ) ;
#1803 = CARTESIAN_POINT ( 'NONE',  ( 73.32203938827501588, 103.9946350594383517, -0.8753108214479579097 ) ) ;
#1804 = ORIENTED_EDGE ( 'NONE', *, *, #20245, .T. ) ;
#1805 = CARTESIAN_POINT ( 'NONE',  ( 49.02192908010439254, 147.4586317741252799, -9.843465619175002956 ) ) ;
#1806 =( BOUNDED_CURVE ( )  B_SPLINE_CURVE ( 2, ( #21685, #11860, #20037, #13516, #20249, #19916, #8567, #4924, #11635, #17029, #6701, #18365, #10326 ),
 .UNSPECIFIED., .F., .F. ) 
 B_SPLINE_CURVE_WITH_KNOTS ( ( 3, 2, 2, 2, 2, 2, 3 ),
 ( 0.06617647058823528106, 0.06764705882352940736, 0.07058823529411764608, 0.07352941176470588480, 0.07647058823529412352, 0.07941176470588234837, 0.08088235294117646079 ),
 .UNSPECIFIED. ) 
 CURVE ( )  GEOMETRIC_REPRESENTATION_ITEM ( )  RATIONAL_B_SPLINE_CURVE ( ( 0.9755282581475765991, 0.9755282581475764880, 1.000000000000000000, 0.9510565162951535312, 1.000000000000000000, 0.9510565162951535312, 1.000000000000000000, 0.9510565162951535312, 1.000000000000000000, 0.9510565162951535312, 1.000000000000000000, 0.9755282581475768211, 0.9755282581475767101 ) ) 
 REPRESENTATION_ITEM ( '' )  );
#1807 = ORIENTED_EDGE ( 'NONE', *, *, #15853, .T. ) ;
#1808 = CARTESIAN_POINT ( 'NONE',  ( 43.01140435219951286, 110.6297705074273097, 29.55568802177586463 ) ) ;
#1809 = CARTESIAN_POINT ( 'NONE',  ( 129.5727795705175822, 84.89323405393692212, 14.00000000000001776 ) ) ;
#1810 = CARTESIAN_POINT ( 'NONE',  ( 39.42975644700377558, 153.4151871740940010, 36.81289934271958941 ) ) ;
#1811 = CARTESIAN_POINT ( 'NONE',  ( 42.00398509169406935, 85.76881261499585207, 8.367275628961508005 ) ) ;
#1812 = CARTESIAN_POINT ( 'NONE',  ( 156.5548063637509415, 177.1359029563629406, -44.99999999999997158 ) ) ;
#1813 = CARTESIAN_POINT ( 'NONE',  ( 147.5268905834513475, 193.0332408774651185, -49.99999999999997158 ) ) ;
#1814 = CARTESIAN_POINT ( 'NONE',  ( -154.5594255724347761, -181.8891397928654783, 59.16757674456785310 ) ) ;
#1815 = CARTESIAN_POINT ( 'NONE',  ( 44.55648932407425633, 101.8104996726487457, 29.45539723777780239 ) ) ;
#1816 = UNCERTAINTY_MEASURE_WITH_UNIT (LENGTH_MEASURE( 1.000000000000000082E-05 ), #4027, 'distance_accuracy_value', 'NONE');
#1817 = CARTESIAN_POINT ( 'NONE',  ( -159.5594255724347761, -194.7891397928654555, 43.77915905869157598 ) ) ;
#1818 = CARTESIAN_POINT ( 'NONE',  ( 46.10157429594899270, 77.66049967264872578, 29.95742577749336988 ) ) ;
#1819 = CARTESIAN_POINT ( 'NONE',  ( 40.27526882409969033, 95.92977050742732104, 30.44471234641811819 ) ) ;
#1820 = CARTESIAN_POINT ( 'NONE',  ( 68.03731475862628031, 132.9047928164914367, -1.867435455408581912 ) ) ;
#1821 = CARTESIAN_POINT ( 'NONE',  ( -154.3824083646099439, -178.2938272943107165, 58.62277379824867296 ) ) ;
#1822 = EDGE_CURVE ( 'NONE', #20771, #7641, #16744, .T. ) ;
#1823 = CARTESIAN_POINT ( 'NONE',  ( 46.59305225739526435, 79.91518717409400097, 31.60846029578754468 ) ) ;
#1824 = CARTESIAN_POINT ( 'NONE',  ( -142.0420953463936087, -195.3938272943107393, 49.65701158161630957 ) ) ;
#1825 = ORIENTED_EDGE ( 'NONE', *, *, #3006, .F. ) ;
#1826 = DIRECTION ( 'NONE',  ( 1.000000000000000000, 0.000000000000000000, 0.000000000000000000 ) ) ;
#1827 = CARTESIAN_POINT ( 'NONE',  ( 28.07864021081662287, 89.10199518432737875, 14.83897397183228861 ) ) ;
#1828 = CARTESIAN_POINT ( 'NONE',  ( 41.64333658814960870, 141.9797705074273324, 38.42115945441014446 ) ) ;
#1829 = CARTESIAN_POINT ( 'NONE',  ( 70.19721620597543676, 127.0927327670264475, -7.624900598222268400 ) ) ;
#1830 = CARTESIAN_POINT ( 'NONE',  ( 38.01140435219952707, 119.6344580088725706, 32.58608133808903773 ) ) ;
#1831 = ORIENTED_EDGE ( 'NONE', *, *, #17120, .T. ) ;
#1832 = CARTESIAN_POINT ( 'NONE',  ( 38.58424406990784661, 147.2297705074273324, 32.77220824515698183 ) ) ;
#1833 = APPLICATION_CONTEXT ( 'automotive_design' ) ;
#1834 = AXIS2_PLACEMENT_3D ( 'NONE', #598, #280, #19122 ) ;
#1835 = CYLINDRICAL_SURFACE ( 'NONE', #10904, 10.00000000000000888 ) ;
#1836 = VECTOR ( 'NONE', #5777, 1000.000000000000000 ) ;
#1837 = EDGE_CURVE ( 'NONE', #5662, #890, #11711, .T. ) ;
#1838 = CARTESIAN_POINT ( 'NONE',  ( 24.43941541943582862, 313.3049502139530205, 4.000000000000003553 ) ) ;
#1839 = CARTESIAN_POINT ( 'NONE',  ( -151.4692556286852891, -196.9891397928655010, 49.65701158161630957 ) ) ;
#1840 = CARTESIAN_POINT ( 'NONE',  ( 26.17254549292281141, -61.68114226949890622, 30.00000000000000000 ) ) ;
#1841 = CARTESIAN_POINT ( 'NONE',  ( 38.96631938032478359, 109.0104996726487485, 37.14960608071593384 ) ) ;
#1842 = CARTESIAN_POINT ( 'NONE',  ( -151.4692556286852891, -165.8130981290892692, 60.17163382399899518 ) ) ;
#1843 =( NAMED_UNIT ( * ) PLANE_ANGLE_UNIT ( ) SI_UNIT ( $, .RADIAN. ) );
#1844 = CARTESIAN_POINT ( 'NONE',  ( 43.01140435219951286, 140.0344580088726048, 28.95336869806222779 ) ) ;
#1845 = CARTESIAN_POINT ( 'NONE',  ( 43.01140435219951286, 125.6297705074273381, 29.55568802177586463 ) ) ;
#1846 = CARTESIAN_POINT ( 'NONE',  ( 50.34320592624661828, 92.59351467088818310, -0.8717445255428065698 ) ) ;
#1847 = DIRECTION ( 'NONE',  ( -0.8660537913735167903, 0.0001295314220487989892, -0.4999508112496346413 ) ) ;
#1848 = CARTESIAN_POINT ( 'NONE',  ( 39.42975644700377558, 117.4151871740940010, 36.81289934271958941 ) ) ;
#1849 = CARTESIAN_POINT ( 'NONE',  ( 137.5268905834513191, 193.0332408774651185, 14.00000000000001776 ) ) ;
#1850 = CARTESIAN_POINT ( 'NONE',  ( 20.25093610150840107, 136.5556286039603435, -4.129180435126924564 ) ) ;
#1851 = FACE_OUTER_BOUND ( 'NONE', #14691, .T. ) ;
#1852 = CARTESIAN_POINT ( 'NONE',  ( 47.43856463449117911, 83.02977050742731535, 32.77220824515697473 ) ) ;
#1853 = VERTEX_POINT ( 'NONE', #14705 ) ;
#1854 = DIRECTION ( 'NONE',  ( 0.000000000000000000, 0.000000000000000000, 1.000000000000000000 ) ) ;
#1855 = CARTESIAN_POINT ( 'NONE',  ( 43.01140435219951286, 69.53445800887257633, 39.46799094044489209 ) ) ;
#1856 = CARTESIAN_POINT ( 'NONE',  ( 116.9721770337685740, 133.1239846058259388, -19.99999999999999289 ) ) ;
#1857 = EDGE_CURVE ( 'NONE', #16415, #13585, #20018, .T. ) ;
#1858 = CARTESIAN_POINT ( 'NONE',  ( 38.01140435219951996, 132.5604996726487457, 32.58608133808903773 ) ) ;
#1860 = CARTESIAN_POINT ( 'NONE',  ( 39.64555921537804295, 153.8934876517313342, -16.27550955686750456 ) ) ;
#1859 = CARTESIAN_POINT ( 'NONE',  ( 46.59305225739526435, 91.91518717409400097, 31.60846029578754468 ) ) ;
#1861 = CARTESIAN_POINT ( 'NONE',  ( -142.0420953463936087, -156.6584106276440593, 49.65701158161630957 ) ) ;
#1862 = CARTESIAN_POINT ( 'NONE',  ( -159.0959885057557983, -185.1938272943107222, 44.11586579668791330 ) ) ;
#1863 = CARTESIAN_POINT ( 'NONE',  ( 41.46631938032478359, 116.1844580088725820, 29.45539723777780239 ) ) ;
#1864 = CARTESIAN_POINT ( 'NONE',  ( 163.1026836591718734, 192.4288937294299160, 34.00000000000001421 ) ) ;
#1865 = DIRECTION ( 'NONE',  ( 0.000000000000000000, 1.000000000000000000, 0.000000000000000000 ) ) ;
#1866 = CARTESIAN_POINT ( 'NONE',  ( -40.97538603781489996, -6.141859983696325465, -25.00000000000000000 ) ) ;
#1867 = CARTESIAN_POINT ( 'NONE',  ( 43.01140435219951286, 155.6297705074273381, 29.55568802177586463 ) ) ;
#1868 = CARTESIAN_POINT ( 'NONE',  ( 43.01140435219951996, 157.4604996726487514, 39.21067981925355639 ) ) ;
#1869 = CARTESIAN_POINT ( 'NONE',  ( 23.42018083028975184, 147.9700754799198705, 17.16443675223517573 ) ) ;
#1870 = CARTESIAN_POINT ( 'NONE',  ( 40.27526882409969744, 141.5651871740940067, 37.97664729208901235 ) ) ;
#1871 = CARTESIAN_POINT ( 'NONE',  ( 43.01140435219957681, 68.03445800887257633, 29.21067981925356705 ) ) ;
#1872 = CARTESIAN_POINT ( 'NONE',  ( -160.8964159109769696, -176.0084106276440536, 52.72008163687743121 ) ) ;
#1873 = CARTESIAN_POINT ( 'NONE',  ( 39.42975644700377558, 59.81518717409399244, 31.60846029578754468 ) ) ;
#1874 = CARTESIAN_POINT ( 'NONE',  ( -148.5561028927606344, -160.2584106276440536, 58.62277379824867296 ) ) ;
#1875 = CARTESIAN_POINT ( 'NONE',  ( 70.23874406963963679, 127.5525917602273012, 4.366313592093098883 ) ) ;
#1876 = DIRECTION ( 'NONE',  ( -0.000000000000000000, -0.000000000000000000, -1.000000000000000000 ) ) ;
#1877 = CARTESIAN_POINT ( 'NONE',  ( 43.01140435219951286, 123.8651871740939896, 38.86567161673127657 ) ) ;
#1878 = VERTEX_POINT ( 'NONE', #4903 ) ;
#1879 = ORIENTED_EDGE ( 'NONE', *, *, #19571, .F. ) ;
#1880 = CARTESIAN_POINT ( 'NONE',  ( 38.96631938032478359, 114.0844580088725877, 37.14960608071593384 ) ) ;
#1881 = ORIENTED_EDGE ( 'NONE', *, *, #2823, .T. ) ;
#1882 = CARTESIAN_POINT ( 'NONE',  ( 41.46631938032478359, 105.3844580088725849, 38.96596240072933170 ) ) ;
#1883 = CARTESIAN_POINT ( 'NONE',  ( 44.55648932407425633, 157.6104996726487570, 38.96596240072933170 ) ) ;
#1885 = CARTESIAN_POINT ( 'NONE',  ( 17.81206540393426252, 132.5069038242342003, 16.68302557436956945 ) ) ;
#1884 = CARTESIAN_POINT ( 'NONE',  ( 38.58424406990784661, 119.9651871740939839, 32.77220824515698183 ) ) ;
#1886 = CARTESIAN_POINT ( 'NONE',  ( 38.01140435219952707, 81.71049967264873715, 34.21067981925357060 ) ) ;
#1887 = CARTESIAN_POINT ( 'NONE',  ( 46.10157429594899270, 147.8344580088725309, 38.46393386101375711 ) ) ;
#1888 = CARTESIAN_POINT ( 'NONE',  ( 43.01140435219951996, 10.71049967264875491, 34.21067981925357060 ) ) ;
#1889 = CARTESIAN_POINT ( 'NONE',  ( -161.4692556286853176, -190.5630981290892976, 49.65701158161630957 ) ) ;
#1890 = CARTESIAN_POINT ( 'NONE',  ( 44.37947211624943833, 82.01518717409400949, 38.42115945441014446 ) ) ;
#1891 = CARTESIAN_POINT ( 'NONE',  ( 41.71002329038685730, 144.8752540357612020, 29.37189892749851694 ) ) ;
#1892 = CARTESIAN_POINT ( 'NONE',  ( 41.46631938032478359, 123.3844580088725849, 38.96596240072933170 ) ) ;
#1893 = CARTESIAN_POINT ( 'NONE',  ( 43.01140435219954838, 131.9604996726487229, 29.21067981925356705 ) ) ;
#1894 = ORIENTED_EDGE ( 'NONE', *, *, #13085, .F. ) ;
#1895 = CARTESIAN_POINT ( 'NONE',  ( -160.8964159109769696, -182.0084106276440821, 52.72008163687743121 ) ) ;
#1896 = CARTESIAN_POINT ( 'NONE',  ( 42.21854335081802390, 85.68333463812091111, 14.36287948008016890 ) ) ;
#1897 = CARTESIAN_POINT ( 'NONE',  ( -148.5561028927606344, -180.0584106276440366, 40.69124936498395328 ) ) ;
#1898 = AXIS2_PLACEMENT_3D ( 'NONE', #17581, #5791, #9447 ) ;
#1899 = ORIENTED_EDGE ( 'NONE', *, *, #8843, .F. ) ;
#1900 = CARTESIAN_POINT ( 'NONE',  ( 40.27526882409969033, 155.6651871740940010, 30.44471234641811819 ) ) ;
#1901 = CARTESIAN_POINT ( 'NONE',  ( 20.98687704487253569, 141.7792436784441747, -11.00219731500033049 ) ) ;
#1902 = CARTESIAN_POINT ( 'NONE',  ( 39.42975644700377558, 117.6797705074273210, 36.81289934271958941 ) ) ;
#1903 = CARTESIAN_POINT ( 'NONE',  ( 46.60148787037231699, 85.86292235506145687, 7.220022382731924537 ) ) ;
#1904 = ORIENTED_EDGE ( 'NONE', *, *, #7576, .F. ) ;
#1905 = VERTEX_POINT ( 'NONE', #7889 ) ;
#1906 = CARTESIAN_POINT ( 'NONE',  ( 47.43856463449118621, 109.8797705074273239, 34.21067981925357060 ) ) ;
#1907 = AXIS2_PLACEMENT_3D ( 'NONE', #20385, #15625, #15526 ) ;
#1908 = FACE_OUTER_BOUND ( 'NONE', #2896, .T. ) ;
#1909 = DIRECTION ( 'NONE',  ( -0.000000000000000000, 1.000000000000000000, -0.000000000000000000 ) ) ;
#1910 = CARTESIAN_POINT ( 'NONE',  ( 40.27526882409969033, 146.6651871740940294, 30.44471234641811819 ) ) ;
#1911 = CARTESIAN_POINT ( 'NONE',  ( 9.468627745026951814, 113.0646104733145592, 1.862908727141013854 ) ) ;
#1912 = CARTESIAN_POINT ( 'NONE',  ( 173.3794444120442506, -34.13255853780189142, 5.000000000000018652 ) ) ;
#1913 = CYLINDRICAL_SURFACE ( 'NONE', #20496, 10.00000000000003730 ) ;
#1914 = EDGE_CURVE ( 'NONE', #10160, #15098, #7604, .T. ) ;
#1915 = CARTESIAN_POINT ( 'NONE',  ( -159.5594255724347761, -170.1891397928654897, 55.53486410454104316 ) ) ;
#1916 = CARTESIAN_POINT ( 'NONE',  ( -161.4692556286852891, -181.4130981290892919, 52.90620854394536821 ) ) ;
#1917 = CARTESIAN_POINT ( 'NONE',  ( 84.42064422693164261, 282.0082918409407284, 272.0939500981630204 ) ) ;
#1918 = CARTESIAN_POINT ( 'NONE',  ( 43.01140435219951286, 91.46049967264873715, 39.21067981925356349 ) ) ;
#1919 = FACE_OUTER_BOUND ( 'NONE', #6043, .T. ) ;
#1920 = CARTESIAN_POINT ( 'NONE',  ( 38.58424406990786082, 96.37977050742732388, 34.21067981925357060 ) ) ;
#1921 = CARTESIAN_POINT ( 'NONE',  ( 55.29376081731632553, 145.2908078538121401, -2.581636314160848489 ) ) ;
#1922 = CARTESIAN_POINT ( 'NONE',  ( -160.8964159109769696, -172.7438272943107336, 52.72008163687743121 ) ) ;
#1923 = VECTOR ( 'NONE', #9629, 1000.000000000000000 ) ;
#1924 = CARTESIAN_POINT ( 'NONE',  ( 47.43856463449118621, 82.61518717409398960, 34.21067981925357060 ) ) ;
#1925 = CARTESIAN_POINT ( 'NONE',  ( -161.4692556286853176, -170.4891397928654726, 49.65701158161630957 ) ) ;
#1926 = CARTESIAN_POINT ( 'NONE',  ( -153.0531000319306827, -159.1622583705452030, 39.65701158161629536 ) ) ;
#1927 = ORIENTED_EDGE ( 'NONE', *, *, #17355, .T. ) ;
#1928 = CARTESIAN_POINT ( 'NONE',  ( 129.5727795705175822, 84.89323405393692212, 4.000000000000021316 ) ) ;
#1929 = CARTESIAN_POINT ( 'NONE',  ( 44.55648932407425633, 121.6104996726487570, 38.96596240072933170 ) ) ;
#1930 =( BOUNDED_CURVE ( )  B_SPLINE_CURVE ( 2, ( #3588, #1926, #8661, #15383, #17126, #277, #7010, #20450, #10422, #5342, #12059, #18791, #15485 ),
 .UNSPECIFIED., .F., .F. ) 
 B_SPLINE_CURVE_WITH_KNOTS ( ( 3, 2, 2, 2, 2, 2, 3 ),
 ( 0.8750000000000000000, 0.8785714285714285587, 0.8857142857142856762, 0.8928571428571429047, 0.9000000000000000222, 0.9071428571428571397, 0.9107142857142856984 ),
 .UNSPECIFIED. ) 
 CURVE ( )  GEOMETRIC_REPRESENTATION_ITEM ( )  RATIONAL_B_SPLINE_CURVE ( ( 0.9755282581475768211, 0.9755282581475768211, 1.000000000000000000, 0.9510565162951535312, 1.000000000000000000, 0.9510565162951535312, 1.000000000000000000, 0.9510565162951535312, 1.000000000000000000, 0.9510565162951535312, 1.000000000000000000, 0.9755282581475768211, 0.9755282581475768211 ) ) 
 REPRESENTATION_ITEM ( '' )  );
#1931 = CARTESIAN_POINT ( 'NONE',  ( 44.37947211624943833, 142.2797705074273154, 38.42115945441014446 ) ) ;
#1932 = CARTESIAN_POINT ( 'NONE',  ( 50.52618006956270591, 153.2232370340747138, -15.91843667049845834 ) ) ;
#1933 = VERTEX_POINT ( 'NONE', #7782 ) ;
#1934 = EDGE_CURVE ( 'NONE', #21705, #12683, #2918, .T. ) ;
#1935 = CARTESIAN_POINT ( 'NONE',  ( 43.01140435219951286, 59.62977050742730967, 29.55568802177586107 ) ) ;
#1936 = EDGE_LOOP ( 'NONE', ( #10832, #15493, #3293, #10748, #3973, #12663, #1527, #9500 ) ) ;
#1937 = CARTESIAN_POINT ( 'NONE',  ( 44.37947211624943833, 137.4797705074273324, 30.00020018409699318 ) ) ;
#1938 = CARTESIAN_POINT ( 'NONE',  ( 38.58424406990786082, 96.37977050742732388, 34.21067981925357060 ) ) ;
#1940 = EDGE_CURVE ( 'NONE', #1193, #13207, #16209, .T. ) ;
#1939 = CARTESIAN_POINT ( 'NONE',  ( 38.96631938032478359, 142.0104996726487627, 37.14960608071593384 ) ) ;
#1941 = DIRECTION ( 'NONE',  ( -0.9385982292947088190, -0.3450121214752277510, 0.000000000000000000 ) ) ;
#1942 = CARTESIAN_POINT ( 'NONE',  ( 43.01140435219951996, 10.71049967264875491, 34.21067981925357060 ) ) ;
#1943 = EDGE_CURVE ( 'NONE', #2795, #13772, #5523, .T. ) ;
#1944 = CARTESIAN_POINT ( 'NONE',  ( 18.86674891209848326, 143.9013856721611546, -11.04182128657428485 ) ) ;
#1945 = CARTESIAN_POINT ( 'NONE',  ( 42.21948215057684450, 109.3836182503284533, 39.21067981925356349 ) ) ;
#1946 = CARTESIAN_POINT ( 'NONE',  ( -151.4692556286852891, -164.3130981290892976, 39.14238933923362396 ) ) ;
#1947 = DIRECTION ( 'NONE',  ( 0.3957342950827466566, 0.000000000000000000, 0.9183650514339936066 ) ) ;
#1948 = VECTOR ( 'NONE', #7134, 1000.000000000000227 ) ;
#1949 = CARTESIAN_POINT ( 'NONE',  ( 38.96631938032478359, 143.4844580088725650, 31.27175355779120025 ) ) ;
#1950 = CARTESIAN_POINT ( 'NONE',  ( 39.42975644700377558, 126.0797705074273267, 31.60846029578754468 ) ) ;
#1951 = CARTESIAN_POINT ( 'NONE',  ( 16.02160000510927418, 128.3529272436884128, 1.509170735004851549 ) ) ;
#1952 = CARTESIAN_POINT ( 'NONE',  ( 48.01140435219951996, 100.1344580088725706, 35.83527830041809636 ) ) ;
#1953 = CARTESIAN_POINT ( 'NONE',  ( 41.64333658814960870, 111.7151871740940123, 38.42115945441014446 ) ) ;
#1954 = CARTESIAN_POINT ( 'NONE',  ( -94.10404323627655288, -13.18023274290474767, 4.000000000000021316 ) ) ;
#1955 = CARTESIAN_POINT ( 'NONE',  ( 30.08091612619420729, 88.20954595054467973, -6.232194961517499188 ) ) ;
#1956 = CARTESIAN_POINT ( 'NONE',  ( 14.81332417359726783, 119.6334487847019403, -4.843746996953559147 ) ) ;
#1957 = CARTESIAN_POINT ( 'NONE',  ( 45.51140435220141001, 58.78519719078001060, 29.88055280033245964 ) ) ;
#1958 = CARTESIAN_POINT ( 'NONE',  ( 38.58424406990785371, 81.52977050742732956, 35.64915139335015937 ) ) ;
#1959 = ORIENTED_EDGE ( 'NONE', *, *, #10473, .T. ) ;
#1960 = AXIS2_PLACEMENT_3D ( 'NONE', #17358, #831, #10968 ) ;
#1961 = EDGE_CURVE ( 'NONE', #19429, #495, #10053, .T. ) ;
#1962 = CARTESIAN_POINT ( 'NONE',  ( 46.10157429594899270, 110.6604996726487400, 29.95742577749336988 ) ) ;
#1963 = CARTESIAN_POINT ( 'NONE',  ( 46.10157429594899270, 73.73445800887257917, 29.95742577749337343 ) ) ;
#1964 = DIRECTION ( 'NONE',  ( 0.000000000000000000, 1.000000000000000000, 0.000000000000000000 ) ) ;
#1965 = CARTESIAN_POINT ( 'NONE',  ( 48.01140435219951996, 134.2104996726487514, 34.21067981925357060 ) ) ;
#1967 = CARTESIAN_POINT ( 'NONE',  ( 20.91795382191701336, 137.2581800298614212, 10.90446256675174297 ) ) ;
#1966 = CARTESIAN_POINT ( 'NONE',  ( 47.43856463449117200, 88.46518717409399812, 35.64915139335016647 ) ) ;
#1968 = CARTESIAN_POINT ( 'NONE',  ( -154.3824083646099439, -157.5584106276440650, 58.62277379824867296 ) ) ;
#1969 = CARTESIAN_POINT ( 'NONE',  ( -160.8964159109769696, -181.8938272943107108, 49.65701158161630957 ) ) ;
#1970 = CARTESIAN_POINT ( 'NONE',  ( -143.3790856849358306, -178.2891397928654840, 55.53486410454105027 ) ) ;
#1971 = CARTESIAN_POINT ( 'NONE',  ( -161.4692556286853176, -193.5630981290892976, 49.65701158161630957 ) ) ;
#1972 = CARTESIAN_POINT ( 'NONE',  ( 48.01140435219951996, 68.36049967264872862, 32.58608133808903773 ) ) ;
#1973 = CARTESIAN_POINT ( 'NONE',  ( -153.0531000319306827, -172.8160212151857138, 59.65701158161631668 ) ) ;
#1974 = CARTESIAN_POINT ( 'NONE',  ( 43.01140435219951286, 148.1297705074272812, 38.86567161673127657 ) ) ;
#1975 = CARTESIAN_POINT ( 'NONE',  ( 41.64333658814960870, 104.7797705074273154, 30.00020018409699318 ) ) ;
#1976 = ADVANCED_FACE ( 'NONE', ( #1372 ), #11393, .T. ) ;
#1977 = CARTESIAN_POINT ( 'NONE',  ( 45.29500579500201951, 154.0643053174194961, 10.91066218119221709 ) ) ;
#1978 = CARTESIAN_POINT ( 'NONE',  ( 43.01140435219951286, 131.3651871740940180, 29.55568802177586107 ) ) ;
#1979 = VECTOR ( 'NONE', #8089, 1000.000000000000000 ) ;
#1980 = CARTESIAN_POINT ( 'NONE',  ( 161.4773229304660731, 84.89323405393692212, -19.99999999999997868 ) ) ;
#1981 = CARTESIAN_POINT ( 'NONE',  ( -159.0959885057557983, -178.8584106276440480, 55.19815736654470584 ) ) ;
#1982 = CARTESIAN_POINT ( 'NONE',  ( 43.01140435219951286, 63.86518717409398960, 38.86567161673127657 ) ) ;
#1983 = CARTESIAN_POINT ( 'NONE',  ( 14.73513546934961482, 119.4163655414939740, 1.151864106104608432 ) ) ;
#1984 = SURFACE_SIDE_STYLE ('',( #20397 ) ) ;
#1985 = CARTESIAN_POINT ( 'NONE',  ( 41.64333658814960870, 111.7151871740940123, 38.42115945441014446 ) ) ;
#1986 = ORIENTED_EDGE ( 'NONE', *, *, #14599, .F. ) ;
#1987 = ORIENTED_EDGE ( 'NONE', *, *, #2982, .T. ) ;
#1988 = FACE_OUTER_BOUND ( 'NONE', #16011, .T. ) ;
#1989 = VERTEX_POINT ( 'NONE', #8104 ) ;
#1990 = CARTESIAN_POINT ( 'NONE',  ( 44.55648932407425633, 105.6844580088725820, 38.96596240072933170 ) ) ;
#1991 = AXIS2_PLACEMENT_3D ( 'NONE', #5809, #10997, #17814 ) ;
#1992 = CARTESIAN_POINT ( 'NONE',  ( 44.37947211624943833, 154.2797705074273438, 38.42115945441014446 ) ) ;
#1993 = CIRCLE ( 'NONE', #19956, 14.42424326798555434 ) ;
#1994 = CARTESIAN_POINT ( 'NONE',  ( 47.05648932407426344, 155.5104996726487343, 31.27175355779120025 ) ) ;
#1996 = CARTESIAN_POINT ( 'NONE',  ( 31.57890723221301599, 145.5991046824261446, -16.55366158474257432 ) ) ;
#1995 = CARTESIAN_POINT ( 'NONE',  ( 44.37947211624943833, 116.2151871740940123, 30.00020018409699318 ) ) ;
#1997 = VECTOR ( 'NONE', #12476, 1000.000000000000000 ) ;
#1998 = CARTESIAN_POINT ( 'NONE',  ( 43.01140435219951286, 73.46049967264872294, 39.46799094044489209 ) ) ;
#2000 = CARTESIAN_POINT ( 'NONE',  ( 38.01140435219952707, 74.63445800887258486, 32.58608133808903773 ) ) ;
#1999 = FACE_OUTER_BOUND ( 'NONE', #9695, .T. ) ;
#2001 = CARTESIAN_POINT ( 'NONE',  ( 38.01140435219952707, 123.7104996726487371, 34.21067981925357060 ) ) ;
#2002 = CARTESIAN_POINT ( 'NONE',  ( 44.62651314315545648, 94.95745790197152303, 38.95396702123348831 ) ) ;
#2003 = CARTESIAN_POINT ( 'NONE',  ( 44.37947211624943833, 74.21518717409399812, 30.00020018409699318 ) ) ;
#2004 = LINE ( 'NONE', #20415, #5529 ) ;
#2005 = CARTESIAN_POINT ( 'NONE',  ( -154.3824083646099439, -185.4938272943107336, 40.69124936498395328 ) ) ;
#2006 = DIRECTION ( 'NONE',  ( 0.000000000000000000, 0.000000000000000000, 1.000000000000000000 ) ) ;
#2007 = ORIENTED_EDGE ( 'NONE', *, *, #6812, .F. ) ;
#2008 = CARTESIAN_POINT ( 'NONE',  ( -143.8425227516148084, -186.9584106276440423, 55.19815736654470584 ) ) ;
#2009 = VECTOR ( 'NONE', #8730, 1000.000000000000000 ) ;
#2010 = CARTESIAN_POINT ( 'NONE',  ( 32.07966263401961982, 152.4337125855422528, -4.522337938825778281 ) ) ;
#2011 = EDGE_CURVE ( 'NONE', #12281, #3209, #3020, .T. ) ;
#2012 = CARTESIAN_POINT ( 'NONE',  ( -157.2955611005346270, -175.7084106276440707, 57.67623309621198047 ) ) ;
#2013 = ORIENTED_EDGE ( 'NONE', *, *, #20527, .F. ) ;
#2014 = CARTESIAN_POINT ( 'NONE',  ( 44.37947211624943833, 146.2151871740940123, 30.00020018409699318 ) ) ;
#2015 = DIRECTION ( 'NONE',  ( -0.000000000000000000, 1.000000000000000000, -0.000000000000000000 ) ) ;
#2016 = CARTESIAN_POINT ( 'NONE',  ( 39.42975644700377558, 102.0797705074273267, 31.60846029578754468 ) ) ;
#2017 = CARTESIAN_POINT ( 'NONE',  ( 17.14282613681034917, 97.48634091255654255, 8.291567264837656381 ) ) ;
#2018 = EDGE_LOOP ( 'NONE', ( #1767, #3911, #17935, #2040 ) ) ;
#2019 = CARTESIAN_POINT ( 'NONE',  ( 15.50679444821833819, 113.6848169819070193, -5.081469017220888063 ) ) ;
#2020 = EDGE_LOOP ( 'NONE', ( #5798, #10588, #11007, #19307 ) ) ;
#2021 = CARTESIAN_POINT ( 'NONE',  ( 41.64333658814960870, 113.7797705074273296, 30.00020018409699318 ) ) ;
#2022 = CARTESIAN_POINT ( 'NONE',  ( 39.92123440845005433, 127.1604996726487542, 38.46393386101375711 ) ) ;
#2023 = CARTESIAN_POINT ( 'NONE',  ( 41.64333658814960870, 149.5151871740940237, 30.00020018409699318 ) ) ;
#2024 = VECTOR ( 'NONE', #19238, 1000.000000000000000 ) ;
#2025 = EDGE_CURVE ( 'NONE', #1195, #13896, #18678, .T. ) ;
#2026 = CARTESIAN_POINT ( 'NONE',  ( 39.92123440845004723, 103.1604996726487258, 38.46393386101376421 ) ) ;
#2027 = CARTESIAN_POINT ( 'NONE',  ( 40.73010619540765020, 85.74955863377461185, -6.589596535617429751 ) ) ;
#2028 = CARTESIAN_POINT ( 'NONE',  ( 43.80332655382220253, 118.5373810949690068, 39.21067981925355639 ) ) ;
#2029 = CARTESIAN_POINT ( 'NONE',  ( -141.4692556286852891, -172.1391397928654783, 52.90620854394536821 ) ) ;
#2030 = DIRECTION ( 'NONE',  ( -0.8510798296367590998, -0.5250363069212118372, 0.000000000000000000 ) ) ;
#2031 = DIRECTION ( 'NONE',  ( 0.3428981916074316239, -0.9393725726208708160, -0.000000000000000000 ) ) ;
#2032 = CYLINDRICAL_SURFACE ( 'NONE', #3445, 27.58651506682278765 ) ;
#2033 = CARTESIAN_POINT ( 'NONE',  ( 46.59305225739526435, 83.17977050742732104, 31.60846029578754468 ) ) ;
#2034 = CARTESIAN_POINT ( 'NONE',  ( 41.15066532084431827, 91.76888749123396849, -6.510040445920065366 ) ) ;
#2035 = CARTESIAN_POINT ( 'NONE',  ( -160.8964159109769696, -178.8938272943107393, 49.65701158161630957 ) ) ;
#2036 = CARTESIAN_POINT ( 'NONE',  ( 38.58424406990786082, 75.11518717409400381, 34.21067981925357060 ) ) ;
#2038 = AXIS2_PLACEMENT_3D ( 'NONE', #18017, #7791, #4796 ) ;
#2037 = DIRECTION ( 'NONE',  ( 0.000000000000000000, 1.000000000000000000, 0.000000000000000000 ) ) ;
#2039 = CARTESIAN_POINT ( 'NONE',  ( -151.4692556286852891, -196.9891397928655010, 59.65701158161632378 ) ) ;
#2040 = ORIENTED_EDGE ( 'NONE', *, *, #6906, .T. ) ;
#2041 = CARTESIAN_POINT ( 'NONE',  ( 126.8576204525573274, -136.9891397928655010, -17.64809332337413750 ) ) ;
#2042 = CARTESIAN_POINT ( 'NONE',  ( -88.69383338279318707, 132.1114735047150646, -19.99999999999996803 ) ) ;
#2043 = CARTESIAN_POINT ( 'NONE',  ( 40.27526882409969744, 140.9297705074273210, 30.44471234641812174 ) ) ;
#2044 = CARTESIAN_POINT ( 'NONE',  ( 21.19424684193554143, 137.6478987072957807, 3.922641511544080917 ) ) ;
#2045 = VERTEX_POINT ( 'NONE', #159 ) ;
#2046 = AXIS2_PLACEMENT_3D ( 'NONE', #16795, #15260, #13597 ) ;
#2047 = ADVANCED_FACE ( 'NONE', ( #15478 ), #18460, .F. ) ;
#2048 = CARTESIAN_POINT ( 'NONE',  ( 134.6380592378699532, 268.5785371414991687, -3.999999999999996447 ) ) ;
#2049 = ORIENTED_EDGE ( 'NONE', *, *, #6385, .T. ) ;
#2050 = CARTESIAN_POINT ( 'NONE',  ( 44.37947211624943833, 133.2797705074273154, 38.42115945441014446 ) ) ;
#2051 = CARTESIAN_POINT ( 'NONE',  ( 40.27526882409969033, 60.56518717409398533, 37.97664729208901946 ) ) ;
#2052 = CARTESIAN_POINT ( 'NONE',  ( 38.58424406990786082, 159.3797705074273381, 34.21067981925357060 ) ) ;
#2053 = PRESENTATION_STYLE_ASSIGNMENT (( #7561 ) ) ;
#2054 = CARTESIAN_POINT ( 'NONE',  ( 47.43856463449117200, 94.46518717409398391, 35.64915139335016647 ) ) ;
#2055 = CARTESIAN_POINT ( 'NONE',  ( 39.92123440845005433, 154.1604996726487400, 38.46393386101375711 ) ) ;
#2056 = LINE ( 'NONE', #11750, #15327 ) ;
#2057 = CARTESIAN_POINT ( 'NONE',  ( -161.4692556286852607, -172.7130981290892464, 46.40781461928724383 ) ) ;
#2058 = CARTESIAN_POINT ( 'NONE',  ( 0.000000000000000000, 0.000000000000000000, 0.000000000000000000 ) ) ;
#2059 = ADVANCED_FACE ( 'NONE', ( #18570 ), #3795, .T. ) ;
#2060 = CARTESIAN_POINT ( 'NONE',  ( 38.01140435219952707, 146.7844580088725763, 34.21067981925357060 ) ) ;
#2061 = B_SPLINE_CURVE_WITH_KNOTS ( 'NONE', 1,
 ( #10082, #20332 ),
 .UNSPECIFIED., .F., .F.,
 ( 2, 2 ),
 ( 0.000000000000000000, 1.000000000000000000 ),
 .UNSPECIFIED. ) ;
#2062 = CARTESIAN_POINT ( 'NONE',  ( 40.27526882409969033, 123.8297705074273125, 37.97664729208901946 ) ) ;
#2063 =( BOUNDED_CURVE ( )  B_SPLINE_CURVE ( 2, ( #15208, #11673, #4731, #19961, #5071, #9927, #3529, #18178, #13445, #14974, #15093, #3308, #3525 ),
 .UNSPECIFIED., .F., .F. ) 
 B_SPLINE_CURVE_WITH_KNOTS ( ( 3, 2, 2, 2, 2, 2, 3 ),
 ( 0.9338235294117647189, 0.9352941176470588314, 0.9382352941176470562, 0.9411764705882352811, 0.9441176470588235059, 0.9470588235294117307, 0.9485294117647058432 ),
 .UNSPECIFIED. ) 
 CURVE ( )  GEOMETRIC_REPRESENTATION_ITEM ( )  RATIONAL_B_SPLINE_CURVE ( ( 0.9755282581475768211, 0.9755282581475768211, 1.000000000000000000, 0.9510565162951535312, 1.000000000000000000, 0.9510565162951535312, 1.000000000000000000, 0.9510565162951535312, 1.000000000000000000, 0.9510565162951535312, 1.000000000000000000, 0.9755282581475768211, 0.9755282581475768211 ) ) 
 REPRESENTATION_ITEM ( '' )  );
#2064 = CARTESIAN_POINT ( 'NONE',  ( 29.98029990418277180, 151.1550010424932111, 23.43402463578956585 ) ) ;
#2065 = CYLINDRICAL_SURFACE ( 'NONE', #12749, 10.00000000000000888 ) ;
#2066 = CARTESIAN_POINT ( 'NONE',  ( 41.64333658814960870, 105.7151871740940123, 38.42115945441014446 ) ) ;
#2067 = CARTESIAN_POINT ( 'NONE',  ( 38.01140435219952707, 125.6344580088725706, 32.58608133808903773 ) ) ;
#2068 = CARTESIAN_POINT ( 'NONE',  ( 64.59149290518072917, 93.33317027722591774, -7.422718449586769296 ) ) ;
#2069 = EDGE_CURVE ( 'NONE', #4207, #6019, #20285, .T. ) ;
#2070 = CARTESIAN_POINT ( 'NONE',  ( 61.33076419740685736, 141.3451534613812441, 11.70407797152743079 ) ) ;
#2071 = FACE_OUTER_BOUND ( 'NONE', #10103, .T. ) ;
#2072 = CARTESIAN_POINT ( 'NONE',  ( 38.58424406990786082, 87.37977050742732388, 34.21067981925357060 ) ) ;
#2073 = ORIENTED_EDGE ( 'NONE', *, *, #13532, .T. ) ;
#2074 = CARTESIAN_POINT ( 'NONE',  ( 48.01140435219951996, 76.43445800887258201, 32.58608133808903773 ) ) ;
#2075 = CARTESIAN_POINT ( 'NONE',  ( -151.4692556286852891, -126.9891397928655010, 59.65701158161632378 ) ) ;
#2076 = CARTESIAN_POINT ( 'NONE',  ( 47.05648932407426344, 133.9104996726487400, 37.14960608071593384 ) ) ;
#2078 = CARTESIAN_POINT ( 'NONE',  ( 73.43285993012185031, 135.4320224564883688, -7.942088354107054826 ) ) ;
#2077 = CARTESIAN_POINT ( 'NONE',  ( 41.64333658814960870, 89.51518717409399528, 30.00020018409699318 ) ) ;
#2079 = CARTESIAN_POINT ( 'NONE',  ( -145.6429501568359797, -160.1084106276440480, 57.67623309621198047 ) ) ;
#2080 = CARTESIAN_POINT ( 'NONE',  ( -157.2955611005345986, -179.3438272943107279, 41.63779006702063867 ) ) ;
#2081 = CARTESIAN_POINT ( 'NONE',  ( 156.5548063637509415, 177.1359029563629406, -44.99999999999997158 ) ) ;
#2082 = DIRECTION ( 'NONE',  ( -1.000000000000000000, 0.000000000000000000, -0.000000000000000000 ) ) ;
#2083 = DIRECTION ( 'NONE',  ( -0.000000000000000000, -0.000000000000000000, -1.000000000000000000 ) ) ;
#2084 = CARTESIAN_POINT ( 'NONE',  ( -151.4692556286853176, -163.7391397928654726, 59.65701158161632378 ) ) ;
#2085 = CARTESIAN_POINT ( 'NONE',  ( 38.58424406990786082, 156.3797705074273097, 34.21067981925357060 ) ) ;
#2086 = CARTESIAN_POINT ( 'NONE',  ( 45.74753988029933538, 101.3297705074273267, 30.44471234641811819 ) ) ;
#2087 = CARTESIAN_POINT ( 'NONE',  ( 14.48810111090402941, 100.9784058478479523, 15.43442115621699529 ) ) ;
#2088 = CARTESIAN_POINT ( 'NONE',  ( 47.43856463449118621, 139.6151871740939896, 34.21067981925357060 ) ) ;
#2089 = DIRECTION ( 'NONE',  ( 1.186952418100008983E-16, 0.000000000000000000, 1.000000000000000000 ) ) ;
#2090 = CARTESIAN_POINT ( 'NONE',  ( -143.8425227516148084, -165.9584106276440423, 55.19815736654470584 ) ) ;
#2091 = CIRCLE ( 'NONE', #15467, 24.99999999999998934 ) ;
#2092 = CARTESIAN_POINT ( 'NONE',  ( 173.3794444120442222, -354.7018910364275257, 19.99999999999999645 ) ) ;
#2093 = CARTESIAN_POINT ( 'NONE',  ( 41.03523200113699687, 148.1191603456353789, 9.842457937073838536 ) ) ;
#2094 = CARTESIAN_POINT ( 'NONE',  ( 40.27526882409969033, 117.5651871740940067, 37.97664729208901946 ) ) ;
#2095 = EDGE_LOOP ( 'NONE', ( #16991, #14494, #15108, #12297 ) ) ;
#2096 = DIRECTION ( 'NONE',  ( -0.3428981916074316239, 0.9393725726208708160, 0.000000000000000000 ) ) ;
#2097 = EDGE_LOOP ( 'NONE', ( #20190, #14115, #19384, #1602, #19878, #10429 ) ) ;
#2098 = CARTESIAN_POINT ( 'NONE',  ( 48.01140435219951996, 100.1344580088725564, 35.83527830041810347 ) ) ;
#2099 = CARTESIAN_POINT ( 'NONE',  ( 38.58424406990784661, 60.52977050742731535, 35.64915139335016647 ) ) ;
#2101 = CARTESIAN_POINT ( 'NONE',  ( 58.92189266798492042, 143.1894642327317513, 11.58510527907202992 ) ) ;
#2100 = CARTESIAN_POINT ( 'NONE',  ( 41.64333658814960870, 119.5151871740940095, 30.00020018409699318 ) ) ;
#2102 = CARTESIAN_POINT ( 'NONE',  ( 38.96631938032478359, 69.41049967264873999, 31.27175355779120025 ) ) ;
#2104 = CARTESIAN_POINT ( 'NONE',  ( -38.21168032741934439, -23.19216891395253910, -19.99999999999997868 ) ) ;
#2103 = CARTESIAN_POINT ( 'NONE',  ( 45.22414464412956647, 144.8093836198929694, 29.72396354041403299 ) ) ;
#2105 = ADVANCED_FACE ( 'NONE', ( #21775 ), #12052, .F. ) ;
#2106 = ADVANCED_FACE ( 'NONE', ( #48, #13498, #17116 ), #16685, .T. ) ;
#2107 = CARTESIAN_POINT ( 'NONE',  ( -157.6495955161842062, -173.0130981290893146, 41.15050349809589392 ) ) ;
#2108 = DIRECTION ( 'NONE',  ( 0.000000000000000000, 0.000000000000000000, 1.000000000000000000 ) ) ;
#2109 = CARTESIAN_POINT ( 'NONE',  ( 41.64333658814960870, 78.71518717409399812, 38.42115945441014446 ) ) ;
#2110 = CARTESIAN_POINT ( 'NONE',  ( 43.01140435219951286, 64.46049967264873715, 39.21067981925356349 ) ) ;
#2111 = CARTESIAN_POINT ( 'NONE',  ( -151.4692556286852891, -179.6438272943107393, 39.74470866294723947 ) ) ;
#2112 = CARTESIAN_POINT ( 'NONE',  ( -157.2955611005345986, -193.7084106276440423, 57.67623309621197336 ) ) ;
#2113 = EDGE_LOOP ( 'NONE', ( #4351, #6041, #11601, #2152 ) ) ;
#2114 = CARTESIAN_POINT ( 'NONE',  ( -159.0959885057557983, -179.4584106276440707, 44.11586579668791330 ) ) ;
#2115 = CARTESIAN_POINT ( 'NONE',  ( 12.43312601512511151, 135.2277911470865490, 16.60371454366222466 ) ) ;
#2116 = VERTEX_POINT ( 'NONE', #8653 ) ;
#2117 = CARTESIAN_POINT ( 'NONE',  ( 40.27526882409969033, 146.6651871740940294, 30.44471234641811819 ) ) ;
#2118 = AXIS2_PLACEMENT_3D ( 'NONE', #18919, #616, #9001 ) ;
#2119 = CARTESIAN_POINT ( 'NONE',  ( 43.01140435219951996, 2.710499672648754466, 9.210679819253577705 ) ) ;
#2120 = CARTESIAN_POINT ( 'NONE',  ( 47.43856463449117911, 107.0297705074273154, 32.77220824515697473 ) ) ;
#2121 = CARTESIAN_POINT ( 'NONE',  ( 30.24639091383375700, 151.6717570033048048, 3.410403464249057492 ) ) ;
#2122 = ORIENTED_EDGE ( 'NONE', *, *, #1202, .F. ) ;
#2123 = CARTESIAN_POINT ( 'NONE',  ( 16.97565887011968400, 109.0741130153051444, 8.727962422049884594 ) ) ;
#2124 = ORIENTED_EDGE ( 'NONE', *, *, #21477, .F. ) ;
#2125 = CARTESIAN_POINT ( 'NONE',  ( 40.27526882409969033, 113.9297705074273068, 30.44471234641811819 ) ) ;
#2126 = CARTESIAN_POINT ( 'NONE',  ( 42.21948215057683740, 158.1113394311928744, 29.21067981925356705 ) ) ;
#2127 = CARTESIAN_POINT ( 'NONE',  ( 38.58424406990786082, 81.37977050742730967, 34.21067981925357060 ) ) ;
#2128 = CARTESIAN_POINT ( 'NONE',  ( 45.74753988029933538, 142.1651871740940010, 37.97664729208901946 ) ) ;
#2129 = CARTESIAN_POINT ( 'NONE',  ( 48.01140435219951996, 104.3604996726487144, 32.58608133808903773 ) ) ;
#2130 = CARTESIAN_POINT ( 'NONE',  ( 17.73005198514846725, 142.9879744078657779, -4.089424278207452801 ) ) ;
#2131 = CLOSED_SHELL ( 'NONE', ( #14070, #2497, #19372, #16215, #5248, #3409, #5840, #17907, #3304, #2907, #15780, #10582, #17008, #14366, #6702 ) ) ;
#2132 = CARTESIAN_POINT ( 'NONE',  ( 20.22230697948889500, 94.36241449208007737, 1.148710122009321211 ) ) ;
#2133 = EDGE_CURVE ( 'NONE', #3147, #7116, #5434, .T. ) ;
#2134 = CARTESIAN_POINT ( 'NONE',  ( 39.92123440845005433, 61.16049967264873288, 38.46393386101375711 ) ) ;
#2135 = CARTESIAN_POINT ( 'NONE',  ( -151.4692556286852891, -168.2391397928654726, 39.14238933923362396 ) ) ;
#2136 = CARTESIAN_POINT ( 'NONE',  ( -151.4692556286852891, -195.2391397928655010, 39.65701158161630246 ) ) ;
#2137 = CARTESIAN_POINT ( 'NONE',  ( 40.73010619540765020, 85.74955863377461185, -6.589596535617429751 ) ) ;
#2138 = LINE ( 'NONE', #9084, #15414 ) ;
#2139 = CARTESIAN_POINT ( 'NONE',  ( 43.01140435219951286, 99.53445800887257633, 39.21067981925356349 ) ) ;
#2140 = CARTESIAN_POINT ( 'NONE',  ( 38.58424406990786082, 84.37977050742730967, 34.21067981925357060 ) ) ;
#2141 = CARTESIAN_POINT ( 'NONE',  ( -145.6429501568359797, -173.9438272943106938, 41.63779006702063867 ) ) ;
#2142 = CARTESIAN_POINT ( 'NONE',  ( 41.64333658814960870, 81.71518717409399812, 38.42115945441014446 ) ) ;
#2143 = DIRECTION ( 'NONE',  ( 0.000000000000000000, -1.000000000000000000, 0.000000000000000000 ) ) ;
#2144 = CARTESIAN_POINT ( 'NONE',  ( 147.5268905834513475, 193.0332408774651185, 4.000000000000021316 ) ) ;
#2145 = ORIENTED_EDGE ( 'NONE', *, *, #9831, .T. ) ;
#2146 = CARTESIAN_POINT ( 'NONE',  ( 38.01140435219952707, 158.7844580088725763, 34.21067981925357060 ) ) ;
#2147 = CARTESIAN_POINT ( 'NONE',  ( -151.4692556286852607, -159.2391397928654726, 39.65701158161629536 ) ) ;
#2148 = CARTESIAN_POINT ( 'NONE',  ( 47.43856463449117911, 137.0297705074272869, 32.77220824515697473 ) ) ;
#2149 = CARTESIAN_POINT ( 'NONE',  ( 75.83902229129397199, 129.3300604911257778, -14.72777435697347137 ) ) ;
#2150 = ORIENTED_EDGE ( 'NONE', *, *, #9010, .T. ) ;
#2151 = FILL_AREA_STYLE_COLOUR ( '', #21717 ) ;
#2152 = ORIENTED_EDGE ( 'NONE', *, *, #1254, .T. ) ;
#2153 = CARTESIAN_POINT ( 'NONE',  ( 44.37947211624943833, 140.4797705074273324, 30.00020018409699318 ) ) ;
#2154 = CARTESIAN_POINT ( 'NONE',  ( 44.37947211624943833, 91.27977050742731535, 38.42115945441014446 ) ) ;
#2155 = CARTESIAN_POINT ( 'NONE',  ( -141.4692556286852891, -180.8391397928654385, 46.40781461928724383 ) ) ;
#2156 = CARTESIAN_POINT ( 'NONE',  ( 41.64333658814960870, 59.51518717409400239, 30.00020018409699318 ) ) ;
#2157 = CARTESIAN_POINT ( 'NONE',  ( 26.17254549292281141, -61.68114226949890622, -46.21320343559645494 ) ) ;
#2158 = CARTESIAN_POINT ( 'NONE',  ( 41.46631938032478359, 159.1104996726487570, 29.45539723777780239 ) ) ;
#2159 = CARTESIAN_POINT ( 'NONE',  ( 38.58424406990784661, 98.96518717409398391, 32.77220824515698183 ) ) ;
#2160 = CARTESIAN_POINT ( 'NONE',  ( 101.4021762516569822, 137.5714195593754710, -35.00000000000000000 ) ) ;
#2161 = CARTESIAN_POINT ( 'NONE',  ( 53.01140435219953417, 119.9070776186055838, -35.00000000000000000 ) ) ;
#2162 = CARTESIAN_POINT ( 'NONE',  ( -145.2889157411863721, -173.6130981290893089, 41.15050349809590102 ) ) ;
#2163 = CARTESIAN_POINT ( 'NONE',  ( 48.01140435219951996, 145.2844580088725763, 34.21067981925357060 ) ) ;
#2164 = CARTESIAN_POINT ( 'NONE',  ( 41.64333658814960870, 116.7797705074273296, 30.00020018409699318 ) ) ;
#2165 = CARTESIAN_POINT ( 'NONE',  ( 70.48772827241290884, 113.2068808858050630, -2.062176545857650201 ) ) ;
#2166 = CARTESIAN_POINT ( 'NONE',  ( 38.58424406990785371, 110.9651871740940123, 32.77220824515697473 ) ) ;
#2167 = ORIENTED_EDGE ( 'NONE', *, *, #19885, .T. ) ;
#2168 = CARTESIAN_POINT ( 'NONE',  ( 180.1254907973641934, 54.87273858953557237, 4.000000000000021316 ) ) ;
#2169 = CARTESIAN_POINT ( 'NONE',  ( 30.38027039762175718, 151.3010018550503446, 11.44158087452429129 ) ) ;
#2170 = CARTESIAN_POINT ( 'NONE',  ( 63.07923660420441792, 139.7192868340247571, 4.799362114056002326 ) ) ;
#2171 = CARTESIAN_POINT ( 'NONE',  ( -141.4692556286852891, -168.8391397928654385, 46.40781461928724383 ) ) ;
#2172 = CIRCLE ( 'NONE', #428, 10.00000000000000888 ) ;
#2173 = VECTOR ( 'NONE', #21757, 1000.000000000000000 ) ;
#2174 = CARTESIAN_POINT ( 'NONE',  ( 38.58424406990785371, 84.52977050742731535, 35.64915139335015937 ) ) ;
#2175 = ORIENTED_EDGE ( 'NONE', *, *, #7095, .T. ) ;
#2176 = CARTESIAN_POINT ( 'NONE',  ( 44.55648932407425633, 61.88445800887257064, 29.45539723777780239 ) ) ;
#2177 = CARTESIAN_POINT ( 'NONE',  ( -151.4692556286852891, -126.9891397928655010, 39.65701158161630246 ) ) ;
#2178 = CARTESIAN_POINT ( 'NONE',  ( 38.01140435219951996, 129.5604996726487457, 32.58608133808903773 ) ) ;
#2180 = CARTESIAN_POINT ( 'NONE',  ( 29.91082003397629663, 88.36561978549612206, -12.22780263974880022 ) ) ;
#2179 = CARTESIAN_POINT ( 'NONE',  ( 40.27526882409969033, 86.66518717409400097, 30.44471234641811819 ) ) ;
#2181 =( BOUNDED_CURVE ( )  B_SPLINE_CURVE ( 2, ( #5019, #15037, #6682, #3477, #15148, #20443, #7003, #15375, #16904, #21776, #13814, #10201, #1918 ),
 .UNSPECIFIED., .F., .T. ) 
 B_SPLINE_CURVE_WITH_KNOTS ( ( 3, 2, 2, 2, 2, 2, 3 ),
 ( 0.6544117647058823595, 0.6558823529411764719, 0.6588235294117646967, 0.6617647058823529216, 0.6647058823529411464, 0.6676470588235293713, 0.6691176470588234837 ),
 .UNSPECIFIED. ) 
 CURVE ( )  GEOMETRIC_REPRESENTATION_ITEM ( )  RATIONAL_B_SPLINE_CURVE ( ( 0.9755282581475768211, 0.9755282581475768211, 1.000000000000000000, 0.9510565162951535312, 1.000000000000000000, 0.9510565162951535312, 1.000000000000000000, 0.9510565162951535312, 1.000000000000000000, 0.9510565162951535312, 1.000000000000000000, 0.9755282581475768211, 0.9755282581475768211 ) ) 
 REPRESENTATION_ITEM ( '' )  );
#2182 = CARTESIAN_POINT ( 'NONE',  ( -151.4692556286852891, -158.9084106276440025, 39.74470866294723947 ) ) ;
#2183 = CARTESIAN_POINT ( 'NONE',  ( -159.0959885057557983, -181.5938272943107279, 55.19815736654470584 ) ) ;
#2184 = CARTESIAN_POINT ( 'NONE',  ( 41.46631938032478359, 94.31049967264874567, 38.96596240072933170 ) ) ;
#2185 = CARTESIAN_POINT ( 'NONE',  ( 44.55648932407425633, 126.6844580088725678, 38.96596240072933170 ) ) ;
#2186 =( NAMED_UNIT ( * ) PLANE_ANGLE_UNIT ( ) SI_UNIT ( $, .RADIAN. ) );
#2187 = VECTOR ( 'NONE', #12158, 1000.000000000000000 ) ;
#2188 = AXIS2_PLACEMENT_3D ( 'NONE', #13387, #4899, #6555 ) ;
#2189 = CARTESIAN_POINT ( 'NONE',  ( 48.01140435219951996, 68.06049967264874567, 35.83527830041809636 ) ) ;
#2190 = CARTESIAN_POINT ( 'NONE',  ( 44.55648932407425633, 143.8104996726487457, 29.45539723777780239 ) ) ;
#2191 = CARTESIAN_POINT ( 'NONE',  ( 47.43856463449117200, 142.7297705074273324, 35.64915139335016647 ) ) ;
#2192 = CARTESIAN_POINT ( 'NONE',  ( 46.59305225739526435, 103.5797705074273267, 36.81289934271958941 ) ) ;
#2193 = CARTESIAN_POINT ( 'NONE',  ( 62.34613790317991544, 148.1570561279473850, 11.50573666851796339 ) ) ;
#2194 = CARTESIAN_POINT ( 'NONE',  ( 44.37947211624943833, 136.0151871740939953, 38.42115945441014446 ) ) ;
#2195 = VECTOR ( 'NONE', #5994, 1000.000000000000000 ) ;
#2196 = DIRECTION ( 'NONE',  ( 0.000000000000000000, 1.000000000000000000, 0.000000000000000000 ) ) ;
#2197 = CARTESIAN_POINT ( 'NONE',  ( -143.8425227516148084, -162.9584106276440423, 55.19815736654470584 ) ) ;
#2198 = CARTESIAN_POINT ( 'NONE',  ( 43.01140435219951286, 67.12977050742732388, 38.86567161673127657 ) ) ;
#2199 = CARTESIAN_POINT ( 'NONE',  ( 0.000000000000000000, -126.9891397928655010, 0.000000000000000000 ) ) ;
#2200 = CARTESIAN_POINT ( 'NONE',  ( 17.32321720400341292, 131.7349665092470730, 8.652027877775747555 ) ) ;
#2201 = DIRECTION ( 'NONE',  ( 0.000000000000000000, -0.000000000000000000, -1.000000000000000000 ) ) ;
#2202 = CARTESIAN_POINT ( 'NONE',  ( 43.01140435219951286, 114.8651871740939754, 38.86567161673127657 ) ) ;
#2203 = VERTEX_POINT ( 'NONE', #3476 ) ;
#2204 = VERTEX_POINT ( 'NONE', #13707 ) ;
#2205 = CARTESIAN_POINT ( 'NONE',  ( 48.01140435219951996, 106.2844580088725763, 34.21067981925357060 ) ) ;
#2206 = CARTESIAN_POINT ( 'NONE',  ( 38.58424406990786082, 147.3797705074273097, 34.21067981925357060 ) ) ;
#2207 = EDGE_CURVE ( 'NONE', #14908, #1684, #11948, .T. ) ;
#2208 = CARTESIAN_POINT ( 'NONE',  ( 47.43856463449118621, 61.87977050742732388, 34.21067981925357060 ) ) ;
#2210 = CARTESIAN_POINT ( 'NONE',  ( 51.29519266978688563, 92.95216133272363379, 14.08499220319455780 ) ) ;
#2209 = CARTESIAN_POINT ( 'NONE',  ( 43.01140435219951286, 119.3651871740939896, 29.55568802177586463 ) ) ;
#2211 = EDGE_CURVE ( 'NONE', #13585, #16648, #10200, .T. ) ;
#2212 = CARTESIAN_POINT ( 'NONE',  ( 48.01140435219951996, 68.06049967264874567, 35.83527830041810347 ) ) ;
#2214 = DIRECTION ( 'NONE',  ( -1.000000000000000000, 0.000000000000000000, 0.000000000000000000 ) ) ;
#2213 = CARTESIAN_POINT ( 'NONE',  ( -136.6255475934131596, 760.1741454933652449, -19.99999999999996092 ) ) ;
#2215 = CARTESIAN_POINT ( 'NONE',  ( 38.01140435219952707, 71.63445800887258486, 32.58608133808903773 ) ) ;
#2216 = CARTESIAN_POINT ( 'NONE',  ( 43.01140435219951286, 94.90707761860558378, 39.21067981925356349 ) ) ;
#2217 = CARTESIAN_POINT ( 'NONE',  ( 41.64333658814960870, 68.51518717409399528, 30.00020018409699318 ) ) ;
#2218 = CARTESIAN_POINT ( 'NONE',  ( 43.01140435219951286, 103.4604996726487371, 39.21067981925356349 ) ) ;
#2219 = CARTESIAN_POINT ( 'NONE',  ( -159.0959885057557983, -178.5938272943107279, 55.19815736654470584 ) ) ;
#2220 = CARTESIAN_POINT ( 'NONE',  ( -151.4692556286852891, -193.4084106276440593, 59.56931450028537256 ) ) ;
#2221 = ORIENTED_EDGE ( 'NONE', *, *, #4577, .F. ) ;
#2222 = CARTESIAN_POINT ( 'NONE',  ( -148.5561028927606344, -178.2584106276440536, 58.62277379824867296 ) ) ;
#2223 = CARTESIAN_POINT ( 'NONE',  ( 61.24245875951225315, 90.83725678726602837, 5.715745788549559059 ) ) ;
#2224 = VERTEX_POINT ( 'NONE', #10307 ) ;
#2225 = CARTESIAN_POINT ( 'NONE',  ( 46.59305225739526435, 142.9151871740940294, 31.60846029578754468 ) ) ;
#2226 = DIRECTION ( 'NONE',  ( 0.000000000000000000, 1.000000000000000000, 0.000000000000000000 ) ) ;
#2227 = CARTESIAN_POINT ( 'NONE',  ( 38.58424406990786082, 102.3797705074273381, 34.21067981925357060 ) ) ;
#2228 = CARTESIAN_POINT ( 'NONE',  ( 29.43094928344231320, 88.48265962617873015, 0.7917390523231137012 ) ) ;
#2229 = ORIENTED_EDGE ( 'NONE', *, *, #20799, .T. ) ;
#2230 = EDGE_CURVE ( 'NONE', #20856, #18762, #16903, .T. ) ;
#2231 = CARTESIAN_POINT ( 'NONE',  ( 69.25106277675128297, 109.5764507715396832, -0.9149236002526208722 ) ) ;
#2232 = ORIENTED_EDGE ( 'NONE', *, *, #18992, .F. ) ;
#2233 = FACE_BOUND ( 'NONE', #12574, .T. ) ;
#2234 = CARTESIAN_POINT ( 'NONE',  ( 46.10157429594899270, 89.66049967264873999, 29.95742577749336988 ) ) ;
#2235 = CARTESIAN_POINT ( 'NONE',  ( 40.27526882409969033, 147.5651871740939498, 37.97664729208901946 ) ) ;
#2236 = CARTESIAN_POINT ( 'NONE',  ( 39.92123440845004723, 105.2604996726487627, 29.95742577749337343 ) ) ;
#2237 = CARTESIAN_POINT ( 'NONE',  ( 76.04618105687035268, 128.8835079444423286, -1.708432735116285350 ) ) ;
#2238 = CARTESIAN_POINT ( 'NONE',  ( 43.01140435219951286, 119.9604996726487229, 29.21067981925356705 ) ) ;
#2239 = CARTESIAN_POINT ( 'NONE',  ( -151.4692556286852891, -172.7391397928655010, 60.17163382399899518 ) ) ;
#2240 = UNCERTAINTY_MEASURE_WITH_UNIT (LENGTH_MEASURE( 1.000000000000000082E-05 ), #9375, 'distance_accuracy_value', 'NONE');
#2241 = CARTESIAN_POINT ( 'NONE',  ( 48.01140435219951996, 64.43445800887258201, 32.58608133808903773 ) ) ;
#2242 = CARTESIAN_POINT ( 'NONE',  ( 43.80332655382220253, 105.6113394311928460, 39.21067981925355639 ) ) ;
#2243 = ORIENTED_EDGE ( 'NONE', *, *, #12450, .T. ) ;
#2244 = CARTESIAN_POINT ( 'NONE',  ( 44.37947211624943833, 86.47977050742731819, 30.00020018409699318 ) ) ;
#2245 = CARTESIAN_POINT ( 'NONE',  ( -142.0420953463935803, -168.5438272943107165, 52.72008163687743831 ) ) ;
#2246 = CARTESIAN_POINT ( 'NONE',  ( 41.64333658814960870, 75.71518717409401233, 38.42115945441014446 ) ) ;
#2247 = CARTESIAN_POINT ( 'NONE',  ( 76.04618105687035268, 128.8835079444423286, -1.708432735116285350 ) ) ;
#2248 = FACE_OUTER_BOUND ( 'NONE', #9607, .T. ) ;
#2249 = ORIENTED_EDGE ( 'NONE', *, *, #16232, .F. ) ;
#2250 = CARTESIAN_POINT ( 'NONE',  ( 38.96631938032478359, 118.0104996726487485, 37.14960608071593384 ) ) ;
#2251 = LINE ( 'NONE', #3913, #13441 ) ;
#2252 = CARTESIAN_POINT ( 'NONE',  ( 47.43856463449117911, 131.0297705074272869, 32.77220824515697473 ) ) ;
#2253 = CARTESIAN_POINT ( 'NONE',  ( 15.21076168709227616, 115.6846582791190201, 9.994193321846964295 ) ) ;
#2254 = ORIENTED_EDGE ( 'NONE', *, *, #72, .F. ) ;
#2255 = PLANE ( 'NONE',  #17823 ) ;
#2256 = ORIENTED_EDGE ( 'NONE', *, *, #305, .F. ) ;
#2257 = CARTESIAN_POINT ( 'NONE',  ( 40.27526882409969033, 132.8297705074273267, 37.97664729208901946 ) ) ;
#2258 = CARTESIAN_POINT ( 'NONE',  ( -151.4692556286852891, -136.9891397928655010, 59.65701158161632378 ) ) ;
#2259 = DIRECTION ( 'NONE',  ( -0.000000000000000000, -1.000000000000000000, -0.000000000000000000 ) ) ;
#2260 = CARTESIAN_POINT ( 'NONE',  ( -141.4692556286852891, -195.0630981290893260, 49.65701158161630957 ) ) ;
#2261 = CARTESIAN_POINT ( 'NONE',  ( 38.58424406990784661, 99.26518717409396686, 35.64915139335016647 ) ) ;
#2262 = CARTESIAN_POINT ( 'NONE',  ( -148.3790856849358306, -174.6630981290893203, 59.16757674456786020 ) ) ;
#2263 = DIRECTION ( 'NONE',  ( 0.000000000000000000, 0.000000000000000000, -1.000000000000000000 ) ) ;
#2264 = CARTESIAN_POINT ( 'NONE',  ( -157.6495955161842062, -157.1130981290892521, 58.16351966513671812 ) ) ;
#2265 = DIRECTION ( 'NONE',  ( 0.000000000000000000, 0.000000000000000000, 1.000000000000000000 ) ) ;
#2266 = CARTESIAN_POINT ( 'NONE',  ( -159.5594255724347761, -191.1891397928654897, 55.53486410454104316 ) ) ;
#2267 = CARTESIAN_POINT ( 'NONE',  ( 48.01140435219951996, 130.4344580088725820, 32.58608133808903773 ) ) ;
#2268 = CARTESIAN_POINT ( 'NONE',  ( 38.58424406990786082, 114.3797705074273097, 34.21067981925357060 ) ) ;
#2269 = CARTESIAN_POINT ( 'NONE',  ( 50.02529374262071826, 147.3041493969045064, 10.19957357710909207 ) ) ;
#2270 = CARTESIAN_POINT ( 'NONE',  ( -159.0959885057557983, -191.1938272943107222, 44.11586579668791330 ) ) ;
#2271 = CARTESIAN_POINT ( 'NONE',  ( 39.42975644700377558, 107.8151871740939924, 31.60846029578754468 ) ) ;
#2272 = VERTEX_POINT ( 'NONE', #15262 ) ;
#2273 = CARTESIAN_POINT ( 'NONE',  ( 9.248697603757472407, 114.7582530722838356, 9.914954709382596931 ) ) ;
#2274 = CARTESIAN_POINT ( 'NONE',  ( 25.64412274706724304, 97.69032544021251852, 15.15625305551708202 ) ) ;
#2275 = ADVANCED_FACE ( 'NONE', ( #20124 ), #17010, .F. ) ;
#2276 = EDGE_CURVE ( 'NONE', #17291, #7232, #14977, .T. ) ;
#2277 = CARTESIAN_POINT ( 'NONE',  ( 44.37947211624943833, 79.27977050742731535, 38.42115945441014446 ) ) ;
#2278 = ORIENTED_EDGE ( 'NONE', *, *, #19182, .T. ) ;
#2279 = CARTESIAN_POINT ( 'NONE',  ( 47.05648932407426344, 63.98445800887257917, 37.14960608071593384 ) ) ;
#2280 = DIRECTION ( 'NONE',  ( 1.000000000000000000, 0.000000000000000000, 0.000000000000000000 ) ) ;
#2281 = CARTESIAN_POINT ( 'NONE',  ( 48.01140435219951996, 125.2104996726487514, 34.21067981925357060 ) ) ;
#2283 = CARTESIAN_POINT ( 'NONE',  ( 46.37776046713125311, 85.92026137128108587, 1.224418530371263580 ) ) ;
#2282 = CARTESIAN_POINT ( 'NONE',  ( 38.58424406990786082, 78.11518717409400381, 34.21067981925357060 ) ) ;
#2284 = ADVANCED_FACE ( 'NONE', ( #1210 ), #7217, .T. ) ;
#2285 = CARTESIAN_POINT ( 'NONE',  ( -160.8964159109769696, -178.8938272943107393, 49.65701158161630957 ) ) ;
#2286 = CARTESIAN_POINT ( 'NONE',  ( 26.66797635711824199, 149.9459070286683868, 17.30505193804556185 ) ) ;
#2287 = CARTESIAN_POINT ( 'NONE',  ( -151.4692556286852891, -192.8130981290892692, 60.17163382399899518 ) ) ;
#2288 = CYLINDRICAL_SURFACE ( 'NONE', #7550, 4.999999999999997335 ) ;
#2289 = CARTESIAN_POINT ( 'NONE',  ( 38.01140435219952707, 158.7844580088725763, 34.21067981925357060 ) ) ;
#2290 = CARTESIAN_POINT ( 'NONE',  ( 41.64333658814960870, 146.7797705074273154, 30.00020018409699318 ) ) ;
#2291 = CARTESIAN_POINT ( 'NONE',  ( 44.37947211624943833, 106.2797705074273154, 38.42115945441014446 ) ) ;
#2292 = CARTESIAN_POINT ( 'NONE',  ( 9.976645104453018220, 110.9295780357170571, 15.79146183154218619 ) ) ;
#2293 = CARTESIAN_POINT ( 'NONE',  ( 41.64333658814960870, 132.7151871740940123, 38.42115945441014446 ) ) ;
#2294 = CARTESIAN_POINT ( 'NONE',  ( 144.5586921005913439, 482.8605407899846682, -19.99999999999999645 ) ) ;
#2295 = CARTESIAN_POINT ( 'NONE',  ( -160.8964159109769696, -161.0084106276440252, 52.72008163687743121 ) ) ;
#2296 = CARTESIAN_POINT ( 'NONE',  ( 39.42975644700377558, 60.67977050742731393, 36.81289934271958941 ) ) ;
#2297 = LINE ( 'NONE', #17284, #12378 ) ;
#2298 = CARTESIAN_POINT ( 'NONE',  ( 47.04142330690687857, 147.8988775214238842, 10.08059930640748902 ) ) ;
#2299 = AXIS2_PLACEMENT_3D ( 'NONE', #9906, #6482, #19938 ) ;
#2300 = CARTESIAN_POINT ( 'NONE',  ( 43.01140435219951996, 2.710499672648754466, 34.21067981925357060 ) ) ;
#2301 = CARTESIAN_POINT ( 'NONE',  ( 44.37947211624943833, 115.0151871740940095, 38.42115945441014446 ) ) ;
#2302 = ORIENTED_EDGE ( 'NONE', *, *, #15475, .F. ) ;
#2303 = PLANE ( 'NONE',  #16261 ) ;
#2304 = EDGE_CURVE ( 'NONE', #15900, #1933, #11111, .T. ) ;
#2305 = ORIENTED_EDGE ( 'NONE', *, *, #5717, .T. ) ;
#2306 =( BOUNDED_SURFACE ( )  B_SPLINE_SURFACE ( 1, 2, ( 
 ( #10356, #10250, #320, #16949, #8594, #15313, #3738, #205, #20384, #17059, #1971, #7049, #10468, #13755, #17168, #2287, #9026, #17812, #21141, #17382, #4267, #14404, #7806, #9348, #19476, #10785, #7377, #10995, #15738, #19156, #19052, #17492, #10678, #17705, #14078, #16164, #5920, #2723, #9464, #2610, #5706, #2505, #1076, #3952, #12648, #749, #14512, #5591, #17599, #6025, #7705, #7484, #19370, #12316, #11099, #14186, #9246, #12756, #20925, #643, #12430, #16052, #2402, #20816, #4057, #5807, #15946, #4368, #12538, #9138, #15838, #962, #19267, #4167, #10896, #856, #7593, #14292, #21037, #1401, #4477, #21356, #6469, #16595, #1513, #10006, #8129, #18372, #2829, #1180, #6589, #14732, #16378, #9790, #21578, #8242, #3274, #6133, #14944, #21691, #11308, #12862, #7915, #14618, #13308, #18262, #14833, #12974, #11205, #21253, #16710, #1619, #19700, #20045, #3165, #4931, #11535, #8351, #9569, #11643, #19583, #17920, #9895, #19923, #6246, #13082, #16275, #19811, #4588, #18035, #2940, #9679, #4700, #11418, #1291, #8026, #13191, #21467, #18143, #6358, #16485, #3052, #4812, #2162, #296, #5042, #405, #7135, #12077, #2057, #8677, #8788, #10547, #11751, #18483, #5461, #15503, #3387, #13731, #13839, #17248, #18808, #20575, #20254, #16820, #20468, #10113, #6815, #6708, #11865, #20149, #5361, #1732, #3819, #15400, #12183, #18918, #3711, #15175, #11974, #15062, #13415, #7027, #10225, #21799, #8467, #5256, #77, #17143, #16927, #10443, #13521, #18596, #3609, #3501, #1842, #8573, #15288, #181, #6916, #13622, #20360, #18703, #10332, #17035, #1946, #2480, #615, #20683, #8899, #12729, #19453, #7351, #4243, #12622, #10969, #21010, #4344, #12290, #17681, #11072, #5568, #19343, #7566, #9000, #726, #2584, #7456, #9324, #16024, #936, #7681, #14163, #20896, #3926, #19135, #9221, #17359, #5783, #14378, #19240, #19028, #7243, #17786, #15919, #10657, #21117, #5999, #5892, #15600, #832, #506, #13945, #2264, #15710, #14056, #20788, #5679, #14264, #12403, #4033, #10759, #17465, #2376, #9113, #15813, #12514, #4140, #10871 ),
 ( #17573, #2807, #21443, #13284, #1049, #3028, #19672, #11622, #6561, #14707, #18238, #4786, #4566, #9764, #20019, #8219, #11287, #6333, #11507, #18007, #16140, #9545, #16461, #14592, #14919, #7783, #1374, #2919, #4678, #13059, #11394, #14483, #16247, #8105, #19900, #3139, #4904, #18117, #21669, #6108, #4451, #9870, #9653, #16354, #1264, #2694, #16569, #9438, #1488, #19785, #21227, #6219, #8000, #14811, #7890, #21554, #11181, #21333, #6445, #12837, #19555, #17894, #12951, #13167, #1156, #3878, #2005, #14004, #458, #10498, #3660, #7189, #5412, #17415, #3987, #12351, #13894, #5313, #10820, #20632, #20738, #12024, #10603, #20525, #10712, #15555, #19087, #20416, #10391, #5627, #15769, #8949, #19192, #2320, #9059, #17091, #7303, #8737, #673, #2432, #18761, #15346, #15455, #355, #12461, #2111, #7083, #7409, #5514, #13682, #239, #12246, #2219, #17198, #12130, #14109, #17522, #13786, #20847, #18863, #5738, #3770, #4089, #18975, #6979, #8848, #17307, #15656, #558, #12899, #21286, #9384, #14218, #19299, #12789, #19620, #2642, #16089, #2757, #9498, #7627, #11344, #16304, #16195, #11237, #19508, #782, #2539, #14329, #9605, #4514, #4401, #1214, #10925, #9171, #21070, #19401, #7948, #4297, #17631, #20958, #14544, #6062, #17957, #21393, #1107, #17847, #2862, #7517, #15869, #14653, #11024, #5842, #12572, #6279, #13011, #4197, #7842, #19732, #18067, #4625, #9276, #5951, #15977, #6165, #888, #12679, #17736, #999, #7736, #14437, #21171, #11132, #3311, #111, #15212, #21818, #3088, #21723, #13549, #1323, #10041, #19964, #11899, #6843, #14978, #18519, #5074, #4849, #16745, #20286, #8499, #11569, #6627, #11788, #18298, #16413, #9821, #1655, #14871, #5180, #8056, #8387, #3200, #11677, #13341, #18411, #14762, #16519, #15096, #20183, #3428, #2974, #6741, #9712, #6392, #4733, #10149, #9930, #16635, #20078, #13449, #16850, #21505, #13120, #1765, #19842, #21616, #11452, #18181, #1435, #8165, #6507, #13227, #1546, #8277, #18627, #650, #7386, #10365, #13977, #536, #20715, #8926, #14086, #215, #5599, #20822, #8601 ) ),
 .UNSPECIFIED., .F., .F., .F. ) 
 B_SPLINE_SURFACE_WITH_KNOTS ( ( 2, 2 ),
 ( 3, 2, 2, 2, 2, 2, 2, 2, 2, 2, 2, 2, 2, 2, 2, 2, 2, 2, 2, 2, 2, 2, 2, 2, 2, 2, 2, 2, 2, 2, 2, 2, 2, 2, 2, 2, 2, 2, 2, 2, 2, 2, 2, 2, 2, 2, 2, 2, 2, 2, 2, 2, 2, 2, 2, 2, 2, 2, 2, 2, 2, 2, 2, 2, 2, 2, 2, 2, 2, 2, 2, 2, 2, 2, 2, 2, 2, 2, 2, 2, 2, 2, 2, 2, 2, 2, 2, 2, 2, 2, 2, 2, 2, 2, 2, 2, 2, 2, 2, 2, 2, 2, 2, 2, 2, 2, 2, 2, 2, 2, 2, 2, 2, 2, 2, 2, 2, 2, 2, 2, 2, 2, 2, 2, 2, 2, 2, 2, 2, 2, 2, 2, 2, 2, 3 ),
 ( 0.000000000000000000, 1.000000000000000000 ),
 ( 0.000000000000000000, 0.007142857142857142634, 0.01428571428571428527, 0.02142857142857142877, 0.02857142857142857054, 0.03571428571428571230, 0.04285714285714285754, 0.05000000000000000278, 0.05714285714285714107, 0.06428571428571427937, 0.07142857142857142461, 0.07857142857142856984, 0.08571428571428571508, 0.09285714285714286031, 0.1000000000000000056, 0.1071428571428571369, 0.1142857142857142821, 0.1214285714285714274, 0.1285714285714285587, 0.1357142857142857040, 0.1428571428571428492, 0.1499999999999999944, 0.1571428571428571397, 0.1642857142857142849, 0.1714285714285714302, 0.1785714285714285754, 0.1857142857142857206, 0.1928571428571428659, 0.2000000000000000111, 0.2071428571428571563, 0.2142857142857142738, 0.2214285714285714191, 0.2285714285714285643, 0.2357142857142857095, 0.2428571428571428548, 0.2500000000000000000, 0.2571428571428571175, 0.2642857142857142905, 0.2714285714285714080, 0.2785714285714285809, 0.2857142857142856984, 0.2928571428571428714, 0.2999999999999999889, 0.3071428571428571619, 0.3142857142857142794, 0.3214285714285714524, 0.3285714285714285698, 0.3357142857142856873, 0.3428571428571428603, 0.3499999999999999778, 0.3571428571428571508, 0.3642857142857142683, 0.3714285714285714413, 0.3785714285714285587, 0.3857142857142857317, 0.3928571428571428492, 0.4000000000000000222, 0.4071428571428571397, 0.4142857142857143127, 0.4214285714285714302, 0.4285714285714285476, 0.4357142857142857206, 0.4428571428571428381, 0.4500000000000000111, 0.4571428571428571286, 0.4642857142857143016, 0.4714285714285714191, 0.4785714285714285920, 0.4857142857142857095, 0.4928571428571428825, 0.5000000000000000000, 0.5071428571428571175, 0.5142857142857142350, 0.5214285714285714635, 0.5285714285714285809, 0.5357142857142856984, 0.5428571428571428159, 0.5500000000000000444, 0.5571428571428571619, 0.5642857142857142794, 0.5714285714285713969, 0.5785714285714286254, 0.5857142857142857428, 0.5928571428571428603, 0.5999999999999999778, 0.6071428571428570953, 0.6142857142857143238, 0.6214285714285714413, 0.6285714285714285587, 0.6357142857142856762, 0.6428571428571429047, 0.6500000000000000222, 0.6571428571428571397, 0.6642857142857142572, 0.6714285714285713746, 0.6785714285714286031, 0.6857142857142857206, 0.6928571428571428381, 0.6999999999999999556, 0.7071428571428571841, 0.7142857142857143016, 0.7214285714285714191, 0.7285714285714285365, 0.7357142857142857650, 0.7428571428571428825, 0.7500000000000000000, 0.7571428571428571175, 0.7642857142857142350, 0.7714285714285714635, 0.7785714285714285809, 0.7857142857142856984, 0.7928571428571428159, 0.8000000000000000444, 0.8071428571428571619, 0.8142857142857142794, 0.8214285714285713969, 0.8285714285714286254, 0.8357142857142857428, 0.8428571428571428603, 0.8499999999999999778, 0.8571428571428570953, 0.8642857142857143238, 0.8714285714285714413, 0.8785714285714285587, 0.8857142857142856762, 0.8928571428571429047, 0.9000000000000000222, 0.9071428571428571397, 0.9142857142857142572, 0.9214285714285713746, 0.9285714285714286031, 0.9357142857142857206, 0.9428571428571428381, 0.9499999999999999556, 0.9523897199067097308 ),
 .UNSPECIFIED. ) 
 GEOMETRIC_REPRESENTATION_ITEM ( )  RATIONAL_B_SPLINE_SURFACE ( (
 ( 1.000000000000000000, 0.9510565162951535312, 1.000000000000000000, 0.9510565162951535312, 1.000000000000000000, 0.9510565162951535312, 1.000000000000000000, 0.9510565162951535312, 1.000000000000000000, 0.9510565162951535312, 1.000000000000000000, 0.9510565162951535312, 1.000000000000000000, 0.9510565162951535312, 1.000000000000000000, 0.9510565162951535312, 1.000000000000000000, 0.9510565162951535312, 1.000000000000000000, 0.9510565162951535312, 1.000000000000000000, 0.9510565162951535312, 1.000000000000000000, 0.9510565162951535312, 1.000000000000000000, 0.9510565162951535312, 1.000000000000000000, 0.9510565162951535312, 1.000000000000000000, 0.9510565162951535312, 1.000000000000000000, 0.9510565162951535312, 1.000000000000000000, 0.9510565162951535312, 1.000000000000000000, 0.9510565162951535312, 1.000000000000000000, 0.9510565162951535312, 1.000000000000000000, 0.9510565162951535312, 1.000000000000000000, 0.9510565162951535312, 1.000000000000000000, 0.9510565162951535312, 1.000000000000000000, 0.9510565162951535312, 1.000000000000000000, 0.9510565162951535312, 1.000000000000000000, 0.9510565162951535312, 1.000000000000000000, 0.9510565162951535312, 1.000000000000000000, 0.9510565162951535312, 1.000000000000000000, 0.9510565162951535312, 1.000000000000000000, 0.9510565162951535312, 1.000000000000000000, 0.9510565162951535312, 1.000000000000000000, 0.9510565162951535312, 1.000000000000000000, 0.9510565162951535312, 1.000000000000000000, 0.9510565162951535312, 1.000000000000000000, 0.9510565162951535312, 1.000000000000000000, 0.9510565162951535312, 1.000000000000000000, 0.9510565162951535312, 1.000000000000000000, 0.9510565162951535312, 1.000000000000000000, 0.9510565162951535312, 1.000000000000000000, 0.9510565162951535312, 1.000000000000000000, 0.9510565162951535312, 1.000000000000000000, 0.9510565162951535312, 1.000000000000000000, 0.9510565162951535312, 1.000000000000000000, 0.9510565162951535312, 1.000000000000000000, 0.9510565162951535312, 1.000000000000000000, 0.9510565162951535312, 1.000000000000000000, 0.9510565162951535312, 1.000000000000000000, 0.9510565162951535312, 1.000000000000000000, 0.9510565162951535312, 1.000000000000000000, 0.9510565162951535312, 1.000000000000000000, 0.9510565162951535312, 1.000000000000000000, 0.9510565162951535312, 1.000000000000000000, 0.9510565162951535312, 1.000000000000000000, 0.9510565162951535312, 1.000000000000000000, 0.9510565162951535312, 1.000000000000000000, 0.9510565162951535312, 1.000000000000000000, 0.9510565162951535312, 1.000000000000000000, 0.9510565162951535312, 1.000000000000000000, 0.9510565162951535312, 1.000000000000000000, 0.9510565162951535312, 1.000000000000000000, 0.9510565162951535312, 1.000000000000000000, 0.9510565162951535312, 1.000000000000000000, 0.9510565162951535312, 1.000000000000000000, 0.9510565162951535312, 1.000000000000000000, 0.9510565162951535312, 1.000000000000000000, 0.9510565162951535312, 1.000000000000000000, 0.9510565162951535312, 1.000000000000000000, 0.9510565162951535312, 1.000000000000000000, 0.9510565162951535312, 1.000000000000000000, 0.9510565162951535312, 1.000000000000000000, 0.9510565162951535312, 1.000000000000000000, 0.9510565162951535312, 1.000000000000000000, 0.9510565162951535312, 1.000000000000000000, 0.9510565162951535312, 1.000000000000000000, 0.9510565162951535312, 1.000000000000000000, 0.9510565162951535312, 1.000000000000000000, 0.9510565162951535312, 1.000000000000000000, 0.9510565162951535312, 1.000000000000000000, 0.9510565162951535312, 1.000000000000000000, 0.9510565162951535312, 1.000000000000000000, 0.9510565162951535312, 1.000000000000000000, 0.9510565162951535312, 1.000000000000000000, 0.9510565162951535312, 1.000000000000000000, 0.9510565162951535312, 1.000000000000000000, 0.9510565162951535312, 1.000000000000000000, 0.9510565162951535312, 1.000000000000000000, 0.9510565162951535312, 1.000000000000000000, 0.9510565162951535312, 1.000000000000000000, 0.9510565162951535312, 1.000000000000000000, 0.9510565162951535312, 1.000000000000000000, 0.9510565162951535312, 1.000000000000000000, 0.9510565162951535312, 1.000000000000000000, 0.9510565162951535312, 1.000000000000000000, 0.9510565162951535312, 1.000000000000000000, 0.9510565162951535312, 1.000000000000000000, 0.9510565162951535312, 1.000000000000000000, 0.9510565162951535312, 1.000000000000000000, 0.9510565162951535312, 1.000000000000000000, 0.9510565162951535312, 1.000000000000000000, 0.9510565162951535312, 1.000000000000000000, 0.9510565162951535312, 1.000000000000000000, 0.9510565162951535312, 1.000000000000000000, 0.9510565162951535312, 1.000000000000000000, 0.9510565162951535312, 1.000000000000000000, 0.9510565162951535312, 1.000000000000000000, 0.9510565162951535312, 1.000000000000000000, 0.9510565162951535312, 1.000000000000000000, 0.9510565162951535312, 1.000000000000000000, 0.9510565162951535312, 1.000000000000000000, 0.9510565162951535312, 1.000000000000000000, 0.9510565162951535312, 1.000000000000000000, 0.9510565162951535312, 1.000000000000000000, 0.9510565162951535312, 1.000000000000000000, 0.9510565162951535312, 1.000000000000000000, 0.9510565162951535312, 1.000000000000000000, 0.9510565162951535312, 1.000000000000000000, 0.9510565162951535312, 1.000000000000000000, 0.9510565162951535312, 1.000000000000000000, 0.9510565162951535312, 1.000000000000000000, 0.9510565162951535312, 1.000000000000000000, 0.9510565162951535312, 1.000000000000000000, 0.9510565162951535312, 1.000000000000000000, 0.9510565162951535312, 1.000000000000000000, 0.9510565162951535312, 1.000000000000000000, 0.9510565162951535312, 1.000000000000000000, 0.9510565162951535312, 1.000000000000000000, 0.9510565162951535312, 1.000000000000000000, 0.9510565162951535312, 1.000000000000000000, 0.9510565162951535312, 1.000000000000000000, 0.9510565162951535312, 1.000000000000000000, 0.9510565162951535312, 1.000000000000000000, 0.9510565162951535312, 1.000000000000000000, 0.9510565162951535312, 1.000000000000000000, 0.9510565162951535312, 1.000000000000000000, 0.9836254295761526212, 0.9782074374858980015),
 ( 1.000000000000000000, 0.9510565162951535312, 1.000000000000000000, 0.9510565162951535312, 1.000000000000000000, 0.9510565162951535312, 1.000000000000000000, 0.9510565162951535312, 1.000000000000000000, 0.9510565162951535312, 1.000000000000000000, 0.9510565162951535312, 1.000000000000000000, 0.9510565162951535312, 1.000000000000000000, 0.9510565162951535312, 1.000000000000000000, 0.9510565162951535312, 1.000000000000000000, 0.9510565162951535312, 1.000000000000000000, 0.9510565162951535312, 1.000000000000000000, 0.9510565162951535312, 1.000000000000000000, 0.9510565162951535312, 1.000000000000000000, 0.9510565162951535312, 1.000000000000000000, 0.9510565162951535312, 1.000000000000000000, 0.9510565162951535312, 1.000000000000000000, 0.9510565162951535312, 1.000000000000000000, 0.9510565162951535312, 1.000000000000000000, 0.9510565162951535312, 1.000000000000000000, 0.9510565162951535312, 1.000000000000000000, 0.9510565162951535312, 1.000000000000000000, 0.9510565162951535312, 1.000000000000000000, 0.9510565162951535312, 1.000000000000000000, 0.9510565162951535312, 1.000000000000000000, 0.9510565162951535312, 1.000000000000000000, 0.9510565162951535312, 1.000000000000000000, 0.9510565162951535312, 1.000000000000000000, 0.9510565162951535312, 1.000000000000000000, 0.9510565162951535312, 1.000000000000000000, 0.9510565162951535312, 1.000000000000000000, 0.9510565162951535312, 1.000000000000000000, 0.9510565162951535312, 1.000000000000000000, 0.9510565162951535312, 1.000000000000000000, 0.9510565162951535312, 1.000000000000000000, 0.9510565162951535312, 1.000000000000000000, 0.9510565162951535312, 1.000000000000000000, 0.9510565162951535312, 1.000000000000000000, 0.9510565162951535312, 1.000000000000000000, 0.9510565162951535312, 1.000000000000000000, 0.9510565162951535312, 1.000000000000000000, 0.9510565162951535312, 1.000000000000000000, 0.9510565162951535312, 1.000000000000000000, 0.9510565162951535312, 1.000000000000000000, 0.9510565162951535312, 1.000000000000000000, 0.9510565162951535312, 1.000000000000000000, 0.9510565162951535312, 1.000000000000000000, 0.9510565162951535312, 1.000000000000000000, 0.9510565162951535312, 1.000000000000000000, 0.9510565162951535312, 1.000000000000000000, 0.9510565162951535312, 1.000000000000000000, 0.9510565162951535312, 1.000000000000000000, 0.9510565162951535312, 1.000000000000000000, 0.9510565162951535312, 1.000000000000000000, 0.9510565162951535312, 1.000000000000000000, 0.9510565162951535312, 1.000000000000000000, 0.9510565162951535312, 1.000000000000000000, 0.9510565162951535312, 1.000000000000000000, 0.9510565162951535312, 1.000000000000000000, 0.9510565162951535312, 1.000000000000000000, 0.9510565162951535312, 1.000000000000000000, 0.9510565162951535312, 1.000000000000000000, 0.9510565162951535312, 1.000000000000000000, 0.9510565162951535312, 1.000000000000000000, 0.9510565162951535312, 1.000000000000000000, 0.9510565162951535312, 1.000000000000000000, 0.9510565162951535312, 1.000000000000000000, 0.9510565162951535312, 1.000000000000000000, 0.9510565162951535312, 1.000000000000000000, 0.9510565162951535312, 1.000000000000000000, 0.9510565162951535312, 1.000000000000000000, 0.9510565162951535312, 1.000000000000000000, 0.9510565162951535312, 1.000000000000000000, 0.9510565162951535312, 1.000000000000000000, 0.9510565162951535312, 1.000000000000000000, 0.9510565162951535312, 1.000000000000000000, 0.9510565162951535312, 1.000000000000000000, 0.9510565162951535312, 1.000000000000000000, 0.9510565162951535312, 1.000000000000000000, 0.9510565162951535312, 1.000000000000000000, 0.9510565162951535312, 1.000000000000000000, 0.9510565162951535312, 1.000000000000000000, 0.9510565162951535312, 1.000000000000000000, 0.9510565162951535312, 1.000000000000000000, 0.9510565162951535312, 1.000000000000000000, 0.9510565162951535312, 1.000000000000000000, 0.9510565162951535312, 1.000000000000000000, 0.9510565162951535312, 1.000000000000000000, 0.9510565162951535312, 1.000000000000000000, 0.9510565162951535312, 1.000000000000000000, 0.9510565162951535312, 1.000000000000000000, 0.9510565162951535312, 1.000000000000000000, 0.9510565162951535312, 1.000000000000000000, 0.9510565162951535312, 1.000000000000000000, 0.9510565162951535312, 1.000000000000000000, 0.9510565162951535312, 1.000000000000000000, 0.9510565162951535312, 1.000000000000000000, 0.9510565162951535312, 1.000000000000000000, 0.9510565162951535312, 1.000000000000000000, 0.9510565162951535312, 1.000000000000000000, 0.9510565162951535312, 1.000000000000000000, 0.9510565162951535312, 1.000000000000000000, 0.9510565162951535312, 1.000000000000000000, 0.9510565162951535312, 1.000000000000000000, 0.9510565162951535312, 1.000000000000000000, 0.9510565162951535312, 1.000000000000000000, 0.9510565162951535312, 1.000000000000000000, 0.9510565162951535312, 1.000000000000000000, 0.9510565162951535312, 1.000000000000000000, 0.9510565162951535312, 1.000000000000000000, 0.9510565162951535312, 1.000000000000000000, 0.9510565162951535312, 1.000000000000000000, 0.9510565162951535312, 1.000000000000000000, 0.9510565162951535312, 1.000000000000000000, 0.9510565162951535312, 1.000000000000000000, 0.9510565162951535312, 1.000000000000000000, 0.9510565162951535312, 1.000000000000000000, 0.9510565162951535312, 1.000000000000000000, 0.9510565162951535312, 1.000000000000000000, 0.9510565162951535312, 1.000000000000000000, 0.9510565162951535312, 1.000000000000000000, 0.9510565162951535312, 1.000000000000000000, 0.9510565162951535312, 1.000000000000000000, 0.9510565162951535312, 1.000000000000000000, 0.9510565162951535312, 1.000000000000000000, 0.9510565162951535312, 1.000000000000000000, 0.9510565162951535312, 1.000000000000000000, 0.9510565162951535312, 1.000000000000000000, 0.9510565162951535312, 1.000000000000000000, 0.9510565162951535312, 1.000000000000000000, 0.9510565162951535312, 1.000000000000000000, 0.9510565162951535312, 1.000000000000000000, 0.9510565162951535312, 1.000000000000000000, 0.9510565162951535312, 1.000000000000000000, 0.9836254295761526212, 0.9782074374858980015) ) ) 
 REPRESENTATION_ITEM ( '' )  SURFACE ( )  );
#2307 = CARTESIAN_POINT ( 'NONE',  ( 38.96631938032478359, 93.08445800887257349, 37.14960608071593384 ) ) ;
#2308 = CARTESIAN_POINT ( 'NONE',  ( 45.74753988029934249, 151.4297705074273210, 37.97664729208901235 ) ) ;
#2309 = CARTESIAN_POINT ( 'NONE',  ( 44.37947211624943833, 59.47977050742732530, 30.00020018409699318 ) ) ;
#2311 = CARTESIAN_POINT ( 'NONE',  ( 24.98902006629997175, 141.4916631675600343, -2.862956674147950409 ) ) ;
#2310 = CARTESIAN_POINT ( 'NONE',  ( 47.43856463449118621, 103.6151871740940038, 34.21067981925357060 ) ) ;
#2312 = CARTESIAN_POINT ( 'NONE',  ( 38.96631938032478359, 76.01049967264873430, 37.14960608071593384 ) ) ;
#2314 = CARTESIAN_POINT ( 'NONE',  ( 48.01140435219951996, 136.2844580088726048, 34.21067981925357060 ) ) ;
#2313 = CARTESIAN_POINT ( 'NONE',  ( 46.31438439993811329, 144.6890179153603242, 30.44285285587857715 ) ) ;
#2315 = FILL_AREA_STYLE ('',( #9166 ) ) ;
#2316 = CIRCLE ( 'NONE', #9711, 4.999999999999997335 ) ;
#2317 = CARTESIAN_POINT ( 'NONE',  ( -151.4692556286852607, -171.8130981290892976, 59.65701158161632378 ) ) ;
#2318 = CARTESIAN_POINT ( 'NONE',  ( 45.51857396895002239, 95.03161353365992170, 38.54896506029344749 ) ) ;
#2319 = DIRECTION ( 'NONE',  ( -1.000000000000000000, 0.000000000000000000, 0.000000000000000000 ) ) ;
#2320 = CARTESIAN_POINT ( 'NONE',  ( -157.2955611005346270, -181.4438272943107506, 57.67623309621198047 ) ) ;
#2321 = CARTESIAN_POINT ( 'NONE',  ( -148.5561028927606344, -190.2584106276440536, 58.62277379824867296 ) ) ;
#2322 = ADVANCED_FACE ( 'NONE', ( #14541 ), #13705, .T. ) ;
#2323 = ORIENTED_EDGE ( 'NONE', *, *, #20650, .F. ) ;
#2324 = CARTESIAN_POINT ( 'NONE',  ( -154.3824083646099439, -175.5584106276440366, 58.62277379824867296 ) ) ;
#2325 = CARTESIAN_POINT ( 'NONE',  ( 69.47322557110069852, 98.06143112153284846, 5.358778726746561638 ) ) ;
#2326 = LINE ( 'NONE', #2647, #3184 ) ;
#2327 = CARTESIAN_POINT ( 'NONE',  ( 44.37947211624943833, 143.2151871740940123, 30.00020018409699318 ) ) ;
#2328 = ADVANCED_FACE ( 'NONE', ( #4870, #11807 ), #14783, .T. ) ;
#2329 = CARTESIAN_POINT ( 'NONE',  ( 40.27526882409969744, 105.8297705074273125, 37.97664729208901235 ) ) ;
#2330 = ORIENTED_EDGE ( 'NONE', *, *, #21000, .T. ) ;
#2331 = ORIENTED_EDGE ( 'NONE', *, *, #10158, .F. ) ;
#2332 = VECTOR ( 'NONE', #19954, 1000.000000000000000 ) ;
#2333 = CARTESIAN_POINT ( 'NONE',  ( 66.10898071834657230, 103.7292514542787245, 6.347102411281516865 ) ) ;
#2334 = CIRCLE ( 'NONE', #19236, 10.00000000000003730 ) ;
#2335 = ORIENTED_EDGE ( 'NONE', *, *, #7205, .T. ) ;
#2336 = CARTESIAN_POINT ( 'NONE',  ( 46.10157429594899270, 114.8344580088725877, 38.46393386101376421 ) ) ;
#2337 = CARTESIAN_POINT ( 'NONE',  ( 39.92123440845005433, 75.26049967264873430, 29.95742577749336988 ) ) ;
#2338 = CARTESIAN_POINT ( 'NONE',  ( 40.27526882409969033, 83.92977050742732104, 30.44471234641811819 ) ) ;
#2339 = CARTESIAN_POINT ( 'NONE',  ( 44.37947211624943833, 143.2151871740940123, 30.00020018409699318 ) ) ;
#2340 = CARTESIAN_POINT ( 'NONE',  ( 39.92123440845004723, 99.26049967264876273, 29.95742577749337343 ) ) ;
#2341 = CARTESIAN_POINT ( 'NONE',  ( 77.19215121279506775, 118.0176990621192203, -1.351406188750652992 ) ) ;
#2342 = CARTESIAN_POINT ( 'NONE',  ( -149.8854112254399240, -179.3899795514095672, 39.65701158161629536 ) ) ;
#2343 = CARTESIAN_POINT ( 'NONE',  ( -148.3790856849358306, -169.5891397928654669, 59.16757674456786020 ) ) ;
#2344 = VECTOR ( 'NONE', #431, 1000.000000000000000 ) ;
#2345 = CARTESIAN_POINT ( 'NONE',  ( 38.96631938032478359, 152.4844580088725934, 31.27175355779120025 ) ) ;
#2346 = DIRECTION ( 'NONE',  ( -0.007125320983191549967, -0.9999746145782334450, 0.000000000000000000 ) ) ;
#2347 = CARTESIAN_POINT ( 'NONE',  ( 44.55648932407425633, 105.6844580088725820, 38.96596240072933170 ) ) ;
#2348 = ADVANCED_FACE ( 'NONE', ( #131 ), #10058, .T. ) ;
#2349 = EDGE_LOOP ( 'NONE', ( #3996, #12011, #2902, #18773, #11925, #10645 ) ) ;
#2350 = STYLED_ITEM ( 'NONE', ( #2362 ), #14370 ) ;
#2351 = CARTESIAN_POINT ( 'NONE',  ( 47.43856463449117200, 88.72977050742730398, 35.64915139335016647 ) ) ;
#2352 = CARTESIAN_POINT ( 'NONE',  ( -145.6429501568359797, -165.8438272943107563, 57.67623309621198047 ) ) ;
#2353 = CARTESIAN_POINT ( 'NONE',  ( 39.42975644700377558, 71.81518717409400665, 31.60846029578754468 ) ) ;
#2354 = CARTESIAN_POINT ( 'NONE',  ( 60.49690154327523572, 149.3382625450468311, -9.565656633516235630 ) ) ;
#2355 = CARTESIAN_POINT ( 'NONE',  ( -142.0420953463936087, -195.6584106276440593, 49.65701158161630957 ) ) ;
#2356 = ORIENTED_EDGE ( 'NONE', *, *, #5717, .F. ) ;
#2357 = CARTESIAN_POINT ( 'NONE',  ( 41.46631938032478359, 117.1104996726487428, 29.45539723777780239 ) ) ;
#2358 = DIRECTION ( 'NONE',  ( 0.000000000000000000, 0.000000000000000000, 1.000000000000000000 ) ) ;
#2359 = CARTESIAN_POINT ( 'NONE',  ( 47.43856463449117911, 136.7297705074273040, 35.64915139335015937 ) ) ;
#2360 = CARTESIAN_POINT ( 'NONE',  ( 32.54106024366770811, 152.4163610972421452, -16.51355214031335805 ) ) ;
#2361 = VERTEX_POINT ( 'NONE', #6415 ) ;
#2362 = PRESENTATION_STYLE_ASSIGNMENT (( #17561 ) ) ;
#2363 = ORIENTED_EDGE ( 'NONE', *, *, #1940, .F. ) ;
#2364 = VECTOR ( 'NONE', #12399, 1000.000000000000000 ) ;
#2365 = CARTESIAN_POINT ( 'NONE',  ( 44.37947211624943833, 136.2797705074273154, 38.42115945441014446 ) ) ;
#2366 = DIRECTION ( 'NONE',  ( 0.000000000000000000, 0.000000000000000000, 1.000000000000000000 ) ) ;
#2367 = CARTESIAN_POINT ( 'NONE',  ( 46.59305225739526435, 92.17977050742732104, 31.60846029578754468 ) ) ;
#2368 = CARTESIAN_POINT ( 'NONE',  ( 164.7397274782390184, 67.46000011932014218, 4.000000000000021316 ) ) ;
#2369 = LINE ( 'NONE', #10754, #11322 ) ;
#2370 = CARTESIAN_POINT ( 'NONE',  ( 38.01140435219952707, 159.7104996726487514, 34.21067981925357060 ) ) ;
#2371 =( BOUNDED_CURVE ( )  B_SPLINE_CURVE ( 2, ( #4987, #8520, #16872, #16656, #15233, #1457, #5203, #14784, #11697, #132, #8296, #6416, #21638 ),
 .UNSPECIFIED., .F., .F. ) 
 B_SPLINE_CURVE_WITH_KNOTS ( ( 3, 2, 2, 2, 2, 2, 3 ),
 ( 0.5535714285714286031, 0.5571428571428571619, 0.5642857142857142794, 0.5714285714285713969, 0.5785714285714286254, 0.5857142857142857428, 0.5892857142857143016 ),
 .UNSPECIFIED. ) 
 CURVE ( )  GEOMETRIC_REPRESENTATION_ITEM ( )  RATIONAL_B_SPLINE_CURVE ( ( 0.9755282581475768211, 0.9755282581475768211, 1.000000000000000000, 0.9510565162951535312, 1.000000000000000000, 0.9510565162951535312, 1.000000000000000000, 0.9510565162951535312, 1.000000000000000000, 0.9510565162951535312, 1.000000000000000000, 0.9755282581475768211, 0.9755282581475768211 ) ) 
 REPRESENTATION_ITEM ( '' )  );
#2372 = AXIS2_PLACEMENT_3D ( 'NONE', #17761, #9738, #18092 ) ;
#2373 = CARTESIAN_POINT ( 'NONE',  ( 47.43856463449118621, 94.61518717409400381, 34.21067981925357060 ) ) ;
#2374 = CARTESIAN_POINT ( 'NONE',  ( 48.01140435219951996, 133.1344580088725706, 35.83527830041809636 ) ) ;
#2375 = CARTESIAN_POINT ( 'NONE',  ( 136.0032066456581674, 182.5367998656340944, 18.98992973508700643 ) ) ;
#2376 = CARTESIAN_POINT ( 'NONE',  ( -145.2889157411863721, -155.6130981290893089, 41.15050349809590102 ) ) ;
#2377 = ADVANCED_FACE ( 'NONE', ( #13468 ), #13138, .F. ) ;
#2378 = CARTESIAN_POINT ( 'NONE',  ( 46.10157429594899270, 70.76049967264873430, 38.46393386101375711 ) ) ;
#2379 = CARTESIAN_POINT ( 'NONE',  ( 39.92123440845004723, 129.2344580088725934, 38.46393386101376421 ) ) ;
#2380 = CARTESIAN_POINT ( 'NONE',  ( 45.74753988029933538, 109.4297705074273210, 37.97664729208901946 ) ) ;
#2381 = CARTESIAN_POINT ( 'NONE',  ( 68.16012629694054681, 106.9699110742356396, 5.199846382127304878 ) ) ;
#2382 = CARTESIAN_POINT ( 'NONE',  ( -159.0959885057557983, -194.1938272943107222, 44.11586579668791330 ) ) ;
#2383 = CARTESIAN_POINT ( 'NONE',  ( 45.74753988029934249, 109.1651871740940010, 37.97664729208901235 ) ) ;
#2384 = AXIS2_PLACEMENT_3D ( 'NONE', #2478, #21008, #4241 ) ;
#2385 = CARTESIAN_POINT ( 'NONE',  ( -149.8854112254399809, -162.7362167067690564, 59.65701158161633089 ) ) ;
#2386 = VERTEX_POINT ( 'NONE', #5094 ) ;
#2387 = CARTESIAN_POINT ( 'NONE',  ( 44.55648932407425633, 156.6844580088725820, 38.96596240072933170 ) ) ;
#2388 = CARTESIAN_POINT ( 'NONE',  ( 74.62708615766334219, 133.0342049366344384, -8.851289726714327344 ) ) ;
#2389 = CARTESIAN_POINT ( 'NONE',  ( 20.99626426110969390, 137.5292218135913913, 9.918250401459649979 ) ) ;
#2390 = FACE_OUTER_BOUND ( 'NONE', #12530, .T. ) ;
#2391 = CARTESIAN_POINT ( 'NONE',  ( 44.37947211624943833, 73.27977050742731535, 38.42115945441014446 ) ) ;
#2392 = ORIENTED_EDGE ( 'NONE', *, *, #15713, .T. ) ;
#2393 = ORIENTED_EDGE ( 'NONE', *, *, #15930, .T. ) ;
#2394 = AXIS2_PLACEMENT_3D ( 'NONE', #3060, #9903, #4940 ) ;
#2395 = CARTESIAN_POINT ( 'NONE',  ( -141.4692556286852891, -165.0630981290893260, 49.65701158161630957 ) ) ;
#2396 = CARTESIAN_POINT ( 'NONE',  ( 47.05648932407426344, 121.9104996726487542, 37.14960608071593384 ) ) ;
#2398 = CARTESIAN_POINT ( 'NONE',  ( 9.127117681521182746, 124.1904119534442401, -3.775300622140596030 ) ) ;
#2397 = CARTESIAN_POINT ( 'NONE',  ( 40.27526882409969033, 80.66518717409400097, 30.44471234641811819 ) ) ;
#2399 = EDGE_CURVE ( 'NONE', #9454, #17720, #16871, .T. ) ;
#2400 = CARTESIAN_POINT ( 'NONE',  ( -159.0959885057557983, -169.5938272943107279, 55.19815736654470584 ) ) ;
#2401 = CARTESIAN_POINT ( 'NONE',  ( 9.231363607564425422, 125.4582397780895633, 16.26765482522027639 ) ) ;
#2402 = CARTESIAN_POINT ( 'NONE',  ( -143.3790856849358306, -185.7630981290893146, 43.77915905869157598 ) ) ;
#2403 = CARTESIAN_POINT ( 'NONE',  ( 0.000000000000000000, 0.000000000000000000, 0.000000000000000000 ) ) ;
#2404 = DIRECTION ( 'NONE',  ( -0.000000000000000000, -0.000000000000000000, 1.000000000000000000 ) ) ;
#2405 = DIRECTION ( 'NONE',  ( 0.000000000000000000, 0.000000000000000000, -1.000000000000000000 ) ) ;
#2406 = CARTESIAN_POINT ( 'NONE',  ( 38.58424406990786082, 138.3797705074273381, 34.21067981925357060 ) ) ;
#2407 = CARTESIAN_POINT ( 'NONE',  ( 77.31131846045057898, 118.9338434746808844, -2.379532457331845485 ) ) ;
#2408 = CARTESIAN_POINT ( 'NONE',  ( 40.27526882409969744, 134.6651871740940010, 30.44471234641812174 ) ) ;
#2409 = CARTESIAN_POINT ( 'NONE',  ( -148.5561028927606344, -168.0584106276440366, 40.69124936498395328 ) ) ;
#2410 = DIRECTION ( 'NONE',  ( 1.387778780781445676E-16, 1.000000000000000000, -0.000000000000000000 ) ) ;
#2411 = CARTESIAN_POINT ( 'NONE',  ( 48.01140435219951996, 91.28445800887257633, 34.21067981925357060 ) ) ;
#2412 = CARTESIAN_POINT ( 'NONE',  ( 14.73996261871784341, 120.6514404024884755, 15.19984638209844441 ) ) ;
#2413 = CARTESIAN_POINT ( 'NONE',  ( 43.01140435219951286, 101.9604996726487371, 29.21067981925356705 ) ) ;
#2414 = CARTESIAN_POINT ( 'NONE',  ( 43.01140435219951286, 117.8651871740939754, 38.86567161673127657 ) ) ;
#2415 = ORIENTED_EDGE ( 'NONE', *, *, #12477, .T. ) ;
#2416 = CARTESIAN_POINT ( 'NONE',  ( 43.01140435219951996, 10.71049967264875491, 34.21067981925357060 ) ) ;
#2417 = VERTEX_POINT ( 'NONE', #18539 ) ;
#2418 = CARTESIAN_POINT ( 'NONE',  ( 41.46631938032478359, 87.38445800887258486, 38.96596240072933170 ) ) ;
#2419 = CARTESIAN_POINT ( 'NONE',  ( 38.58424406990785371, 150.2297705074273040, 32.77220824515697473 ) ) ;
#2420 = CARTESIAN_POINT ( 'NONE',  ( 43.01140435219951286, 145.4604996726487229, 39.46799094044489209 ) ) ;
#2422 = CARTESIAN_POINT ( 'NONE',  ( 70.19721620597543676, 127.0927327670264475, -7.624900598222268400 ) ) ;
#2421 = CARTESIAN_POINT ( 'NONE',  ( 44.37947211624943833, 103.0151871740939953, 38.42115945441014446 ) ) ;
#2423 = CARTESIAN_POINT ( 'NONE',  ( 47.05648932407426344, 76.91049967264873999, 37.14960608071593384 ) ) ;
#2425 = CARTESIAN_POINT ( 'NONE',  ( 48.01140435219951996, 61.28445800887258343, 34.21067981925357060 ) ) ;
#2424 = DIRECTION ( 'NONE',  ( 0.9385982292947088190, 0.3450121214752278620, -0.000000000000000000 ) ) ;
#2426 = CARTESIAN_POINT ( 'NONE',  ( 43.01140435219951996, 10.71049967264875491, 39.21067981925356349 ) ) ;
#2427 = VECTOR ( 'NONE', #15194, 1000.000000000000000 ) ;
#2428 = CARTESIAN_POINT ( 'NONE',  ( 43.01140435219951996, 10.71049967264875491, 34.21067981925357060 ) ) ;
#2429 = CARTESIAN_POINT ( 'NONE',  ( -154.5594255724347761, -189.9630981290893317, 59.16757674456785310 ) ) ;
#2430 = CARTESIAN_POINT ( 'NONE',  ( 40.27526882409969033, 66.56518717409400665, 37.97664729208901946 ) ) ;
#2431 = DIRECTION ( 'NONE',  ( 0.000000000000000000, 1.000000000000000000, 0.000000000000000000 ) ) ;
#2432 = CARTESIAN_POINT ( 'NONE',  ( -142.0420953463935803, -180.5438272943106881, 52.72008163687743831 ) ) ;
#2433 = CARTESIAN_POINT ( 'NONE',  ( 173.3794444120442506, -34.13255853780189142, 5.000000000000018652 ) ) ;
#2434 = ORIENTED_EDGE ( 'NONE', *, *, #13221, .T. ) ;
#2435 = CARTESIAN_POINT ( 'NONE',  ( 29.59780345622613851, 88.32329120701308511, 6.787350155335245994 ) ) ;
#2436 = EDGE_LOOP ( 'NONE', ( #12164, #19467, #16101, #7360, #18553, #14229, #20531, #9668 ) ) ;
#2437 = CARTESIAN_POINT ( 'NONE',  ( 38.58424406990784661, 144.2651871740940237, 35.64915139335016647 ) ) ;
#2438 = CARTESIAN_POINT ( 'NONE',  ( 41.64333658814960870, 104.7797705074273154, 30.00020018409699318 ) ) ;
#2439 = VERTEX_POINT ( 'NONE', #16766 ) ;
#2440 = ORIENTED_EDGE ( 'NONE', *, *, #14295, .F. ) ;
#2441 = CARTESIAN_POINT ( 'NONE',  ( 70.84063976188440392, 115.3547488198113200, -1.153064885589385025 ) ) ;
#2442 = ADVANCED_FACE ( 'NONE', ( #15116 ), #3447, .T. ) ;
#2443 = ORIENTED_EDGE ( 'NONE', *, *, #20870, .T. ) ;
#2444 = CARTESIAN_POINT ( 'NONE',  ( 47.05648932407426344, 114.9844580088725792, 37.14960608071593384 ) ) ;
#2445 = CARTESIAN_POINT ( 'NONE',  ( 135.5718357590524192, 174.6787949867965324, 4.000000000000021316 ) ) ;
#2446 = CARTESIAN_POINT ( 'NONE',  ( 38.58424406990784661, 75.22977050742730398, 32.77220824515698183 ) ) ;
#2447 = CARTESIAN_POINT ( 'NONE',  ( 46.59305225739526435, 136.9151871740940010, 31.60846029578754468 ) ) ;
#2448 = CARTESIAN_POINT ( 'NONE',  ( 38.01140435219951996, 105.5604996726487173, 32.58608133808903773 ) ) ;
#2449 = CARTESIAN_POINT ( 'NONE',  ( 45.29500579500201951, 154.0643053174194961, 10.91066218119221709 ) ) ;
#2450 = CARTESIAN_POINT ( 'NONE',  ( -143.3790856849358306, -180.3630981290893089, 55.53486410454105027 ) ) ;
#2451 = CARTESIAN_POINT ( 'NONE',  ( -154.5594255724347761, -159.0891397928654953, 40.14644641866476604 ) ) ;
#2452 = DIRECTION ( 'NONE',  ( 1.000000000000000000, 0.000000000000000000, -1.723963091245776585E-16 ) ) ;
#2453 = LINE ( 'NONE', #16000, #13982 ) ;
#2454 = CARTESIAN_POINT ( 'NONE',  ( 43.01140435219951996, 10.71049967264875491, 34.21067981925357060 ) ) ;
#2455 =( GEOMETRIC_REPRESENTATION_CONTEXT ( 3 ) GLOBAL_UNCERTAINTY_ASSIGNED_CONTEXT ( ( #3580 ) ) GLOBAL_UNIT_ASSIGNED_CONTEXT ( ( #3502, #19924, #18484 ) ) REPRESENTATION_CONTEXT ( 'NONE', 'WORKASPACE' ) );
#2456 = ORIENTED_EDGE ( 'NONE', *, *, #8916, .F. ) ;
#2457 = CARTESIAN_POINT ( 'NONE',  ( 41.64333658814960870, 87.97977050742731819, 38.42115945441014446 ) ) ;
#2458 = CARTESIAN_POINT ( 'NONE',  ( -148.5561028927606344, -167.7938272943107165, 40.69124936498395328 ) ) ;
#2459 = CARTESIAN_POINT ( 'NONE',  ( 44.41273964558330789, 85.70220254879866673, -6.708519844216274564 ) ) ;
#2460 = CARTESIAN_POINT ( 'NONE',  ( -151.4692556286852891, -191.9084106276440025, 39.74470866294723947 ) ) ;
#2461 = ORIENTED_EDGE ( 'NONE', *, *, #21477, .T. ) ;
#2462 = CARTESIAN_POINT ( 'NONE',  ( -161.4692556286853176, -175.5630981290893260, 49.65701158161630957 ) ) ;
#2463 = CARTESIAN_POINT ( 'NONE',  ( 138.2733499813809885, 177.2661675079481540, -29.99999999999997868 ) ) ;
#2464 = CARTESIAN_POINT ( 'NONE',  ( 40.27526882409969744, 137.9297705074273210, 30.44471234641812174 ) ) ;
#2465 = CARTESIAN_POINT ( 'NONE',  ( 57.55288598684787615, 89.00415807515548750, -6.156345639627279986 ) ) ;
#2466 = ORIENTED_EDGE ( 'NONE', *, *, #13663, .T. ) ;
#2467 = DIRECTION ( 'NONE',  ( 0.000000000000000000, 0.000000000000000000, -1.000000000000000000 ) ) ;
#2468 = EDGE_LOOP ( 'NONE', ( #13014, #8962, #5399, #8911 ) ) ;
#2469 = CARTESIAN_POINT ( 'NONE',  ( 39.42975644700377558, 123.6797705074273210, 36.81289934271958941 ) ) ;
#2470 = CARTESIAN_POINT ( 'NONE',  ( 46.10157429594899270, 138.8344580088725877, 38.46393386101375711 ) ) ;
#2471 = CIRCLE ( 'NONE', #12318, 27.14138364107347812 ) ;
#2472 = CARTESIAN_POINT ( 'NONE',  ( 46.10157429594899270, 155.6604996726487116, 29.95742577749336988 ) ) ;
#2473 = ADVANCED_FACE ( 'NONE', ( #13359 ), #13030, .F. ) ;
#2474 = DIRECTION ( 'NONE',  ( 0.000000000000000000, 1.000000000000000000, 0.000000000000000000 ) ) ;
#2475 = DIRECTION ( 'NONE',  ( 0.000000000000000000, 1.000000000000000000, 0.000000000000000000 ) ) ;
#2476 = EDGE_CURVE ( 'NONE', #1878, #10563, #4648, .T. ) ;
#2477 = CARTESIAN_POINT ( 'NONE',  ( 44.37947211624943833, 100.0151871740939953, 38.42115945441014446 ) ) ;
#2478 = CARTESIAN_POINT ( 'NONE',  ( 43.01140435219951996, 119.9070776186055838, -35.00000000000000000 ) ) ;
#2479 = DIRECTION ( 'NONE',  ( -0.000000000000000000, -0.000000000000000000, 1.000000000000000000 ) ) ;
#2480 = CARTESIAN_POINT ( 'NONE',  ( -154.5594255724347761, -164.1630981290892919, 40.14644641866476604 ) ) ;
#2481 = CARTESIAN_POINT ( 'NONE',  ( 43.01140435219957681, 71.96049967264872294, 29.21067981925356705 ) ) ;
#2482 = CARTESIAN_POINT ( 'NONE',  ( 39.92123440845004723, 137.3344580088725593, 29.95742577749337343 ) ) ;
#2483 = CARTESIAN_POINT ( 'NONE',  ( 39.42975644700377558, 114.0797705074273125, 31.60846029578754468 ) ) ;
#2484 = CARTESIAN_POINT ( 'NONE',  ( 71.26135857449716582, 118.5824631887579272, 4.723566274445706092 ) ) ;
#2485 = CARTESIAN_POINT ( 'NONE',  ( -148.5561028927606344, -191.7938272943107449, 40.69124936498395328 ) ) ;
#2486 = CARTESIAN_POINT ( 'NONE',  ( 45.74753988029934249, 95.06518717409399244, 30.44471234641812174 ) ) ;
#2487 = CYLINDRICAL_SURFACE ( 'NONE', #17723, 10.00000000000000888 ) ;
#2488 = ORIENTED_EDGE ( 'NONE', *, *, #1675, .F. ) ;
#2489 = AXIS2_PLACEMENT_3D ( 'NONE', #220, #19066, #12443 ) ;
#2490 = CARTESIAN_POINT ( 'NONE',  ( 43.80332655382220253, 76.95757658655229250, 29.21067981925356705 ) ) ;
#2491 = CARTESIAN_POINT ( 'NONE',  ( 73.32203938827501588, 103.9946350594383517, -0.8753108214479579097 ) ) ;
#2492 = CARTESIAN_POINT ( 'NONE',  ( 69.68673170630326297, 129.0522134326295145, 12.29911014595921692 ) ) ;
#2493 = CARTESIAN_POINT ( 'NONE',  ( 43.80332655382220253, 154.9575765865523067, 29.21067981925356705 ) ) ;
#2494 = CARTESIAN_POINT ( 'NONE',  ( 43.01140435219951286, 80.62977050742732388, 29.55568802177586107 ) ) ;
#2495 = ORIENTED_EDGE ( 'NONE', *, *, #12654, .T. ) ;
#2496 = DIRECTION ( 'NONE',  ( -0.000000000000000000, -0.000000000000000000, 1.000000000000000000 ) ) ;
#2497 = ADVANCED_FACE ( 'NONE', ( #6651 ), #18088, .F. ) ;
#2498 =( BOUNDED_CURVE ( )  B_SPLINE_CURVE ( 2, ( #10653, #15499, #401, #5778, #5456, #9217, #15915, #4135, #7239, #825, #18912, #10544, #17244 ),
 .UNSPECIFIED., .F., .F. ) 
 B_SPLINE_CURVE_WITH_KNOTS ( ( 3, 2, 2, 2, 2, 2, 3 ),
 ( 0.05357142857142858927, 0.05714285714285714107, 0.06428571428571427937, 0.07142857142857142461, 0.07857142857142856984, 0.08571428571428571508, 0.08928571428571425994 ),
 .UNSPECIFIED. ) 
 CURVE ( )  GEOMETRIC_REPRESENTATION_ITEM ( )  RATIONAL_B_SPLINE_CURVE ( ( 0.9755282581475767101, 0.9755282581475768211, 1.000000000000000000, 0.9510565162951535312, 1.000000000000000000, 0.9510565162951535312, 1.000000000000000000, 0.9510565162951535312, 1.000000000000000000, 0.9510565162951535312, 1.000000000000000000, 0.9755282581475769321, 0.9755282581475768211 ) ) 
 REPRESENTATION_ITEM ( '' )  );
#2499 = LINE ( 'NONE', #743, #5251 ) ;
#2500 = CARTESIAN_POINT ( 'NONE',  ( 38.01140435219951996, 120.8604996726487428, 35.83527830041810347 ) ) ;
#2502 = CARTESIAN_POINT ( 'NONE',  ( 76.87285023715404009, 124.3600315475450486, -0.5611826874715375446 ) ) ;
#2501 = CARTESIAN_POINT ( 'NONE',  ( 46.59305225739526435, 73.91518717409400097, 31.60846029578754468 ) ) ;
#2503 = CARTESIAN_POINT ( 'NONE',  ( -142.0420953463936087, -174.3938272943107393, 49.65701158161630957 ) ) ;
#2504 = CARTESIAN_POINT ( 'NONE',  ( 12.43312601512511151, 135.2277911470865490, 16.60371454366222466 ) ) ;
#2505 = CARTESIAN_POINT ( 'NONE',  ( -141.4692556286852891, -188.9130981290893487, 46.40781461928724383 ) ) ;
#2506 =( NAMED_UNIT ( * ) PLANE_ANGLE_UNIT ( ) SI_UNIT ( $, .RADIAN. ) );
#2507 = LINE ( 'NONE', #19268, #16704 ) ;
#2508 = CARTESIAN_POINT ( 'NONE',  ( -145.2889157411863437, -162.5391397928654271, 41.15050349809589392 ) ) ;
#2509 = CARTESIAN_POINT ( 'NONE',  ( 40.27526882409969033, 141.8297705074273267, 37.97664729208901946 ) ) ;
#2510 = CARTESIAN_POINT ( 'NONE',  ( 9.433072040199128594, 112.8364229897773470, 7.858512901693939234 ) ) ;
#2511 = CARTESIAN_POINT ( 'NONE',  ( 39.42975644700377558, 126.4151871740940010, 36.81289934271958941 ) ) ;
#2512 = SURFACE_STYLE_FILL_AREA ( #970 ) ;
#2513 = CARTESIAN_POINT ( 'NONE',  ( -148.5561028927606344, -165.0584106276440366, 40.69124936498395328 ) ) ;
#2514 = CARTESIAN_POINT ( 'NONE',  ( 43.01140435219951286, 59.62977050742730967, 29.55568802177586463 ) ) ;
#2515 = DIRECTION ( 'NONE',  ( -1.000000000000000000, 0.000000000000000000, 0.000000000000000000 ) ) ;
#2516 = CARTESIAN_POINT ( 'NONE',  ( 21.79768317403592803, 101.2052074350461339, 14.36631359211887649 ) ) ;
#2517 = CYLINDRICAL_SURFACE ( 'NONE', #19740, 4.999999999999997335 ) ;
#2518 = CARTESIAN_POINT ( 'NONE',  ( 38.58424406990786082, 108.1151871740940038, 34.21067981925357060 ) ) ;
#2519 = ORIENTED_EDGE ( 'NONE', *, *, #2728, .T. ) ;
#2520 = EDGE_CURVE ( 'NONE', #2224, #7555, #21637, .T. ) ;
#2521 = CARTESIAN_POINT ( 'NONE',  ( -143.3790856849358306, -157.2891397928654555, 55.53486410454105027 ) ) ;
#2522 = ORIENTED_EDGE ( 'NONE', *, *, #3156, .F. ) ;
#2523 = CARTESIAN_POINT ( 'NONE',  ( 41.46631938032478359, 92.18445800887258201, 29.45539723777780239 ) ) ;
#2524 = CARTESIAN_POINT ( 'NONE',  ( 46.59305225739526435, 149.1797705074273210, 31.60846029578754468 ) ) ;
#2525 = VECTOR ( 'NONE', #1351, 1000.000000000000000 ) ;
#2526 =( REPRESENTATION_RELATIONSHIP ('NONE','NONE', #6933, #3970 ) REPRESENTATION_RELATIONSHIP_WITH_TRANSFORMATION ( #14708 )SHAPE_REPRESENTATION_RELATIONSHIP( ) );
#2527 = AXIS2_PLACEMENT_3D ( 'NONE', #10957, #17666, #9308 ) ;
#2528 = CARTESIAN_POINT ( 'NONE',  ( 41.46631938032478359, 145.3104996726487457, 38.96596240072933170 ) ) ;
#2530 = CARTESIAN_POINT ( 'NONE',  ( 20.44379504597808861, 136.6827000062168338, -10.12478428749056469 ) ) ;
#2529 = CARTESIAN_POINT ( 'NONE',  ( 38.58424406990784661, 104.9651871740940123, 32.77220824515698183 ) ) ;
#2531 = CARTESIAN_POINT ( 'NONE',  ( 43.01140435219951996, 10.71049967264875491, 29.21067981925357060 ) ) ;
#2533 = DIRECTION ( 'NONE',  ( 0.000000000000000000, 0.000000000000000000, 1.000000000000000000 ) ) ;
#2532 = CARTESIAN_POINT ( 'NONE',  ( 44.63189717924443300, 144.8563245053103401, 38.95199156105033467 ) ) ;
#2534 = SURFACE_SIDE_STYLE ('',( #15865 ) ) ;
#2535 = CARTESIAN_POINT ( 'NONE',  ( -166.4803626276155626, -116.9891397928655010, 49.65701158161629536 ) ) ;
#2536 = CARTESIAN_POINT ( 'NONE',  ( -176.9699209214867892, 72.84679049016739327, -19.99999999999995737 ) ) ;
#2537 = CARTESIAN_POINT ( 'NONE',  ( 44.41273964558330789, 85.70220254879866673, -6.708519844216274564 ) ) ;
#2538 = CARTESIAN_POINT ( 'NONE',  ( 162.0641828542163125, 116.7231784796025948, -19.99999999999997868 ) ) ;
#2539 = CARTESIAN_POINT ( 'NONE',  ( -157.2955611005346270, -173.3438272943107279, 41.63779006702063867 ) ) ;
#2540 = CARTESIAN_POINT ( 'NONE',  ( -159.0959885057557983, -191.4584106276440423, 44.11586579668791330 ) ) ;
#2541 = ORIENTED_EDGE ( 'NONE', *, *, #10210, .T. ) ;
#2542 = CARTESIAN_POINT ( 'NONE',  ( -142.0420953463936087, -177.6584106276440309, 49.65701158161630957 ) ) ;
#2543 = CARTESIAN_POINT ( 'NONE',  ( 47.27474595639033339, 153.9548969447091906, 2.977729283044022957 ) ) ;
#2544 = FACE_OUTER_BOUND ( 'NONE', #1416, .T. ) ;
#2545 = CARTESIAN_POINT ( 'NONE',  ( 39.42975644700377558, 138.4151871740940010, 36.81289934271958941 ) ) ;
#2546 = CARTESIAN_POINT ( 'NONE',  ( 40.27526882409969744, 98.92977050742732104, 30.44471234641812174 ) ) ;
#2547 = ORIENTED_EDGE ( 'NONE', *, *, #1784, .F. ) ;
#2548 = VERTEX_POINT ( 'NONE', #16654 ) ;
#2549 = EDGE_CURVE ( 'NONE', #15790, #784, #8294, .T. ) ;
#2550 = CARTESIAN_POINT ( 'NONE',  ( 58.43892221570314405, 143.5117748958429047, 4.561220828673259398 ) ) ;
#2551 = ORIENTED_EDGE ( 'NONE', *, *, #8145, .T. ) ;
#2552 = CARTESIAN_POINT ( 'NONE',  ( 48.01140435219951996, 112.4344580088725678, 32.58608133808903773 ) ) ;
#2553 = CARTESIAN_POINT ( 'NONE',  ( 38.01140435219952707, 75.56049967264873146, 32.58608133808903773 ) ) ;
#2554 = CARTESIAN_POINT ( 'NONE',  ( 45.74753988029933538, 76.42977050742729261, 37.97664729208901946 ) ) ;
#2555 = CARTESIAN_POINT ( 'NONE',  ( 38.58424406990784661, 132.2651871740939953, 35.64915139335016647 ) ) ;
#2556 = CARTESIAN_POINT ( 'NONE',  ( 38.96631938032478359, 93.41049967264873999, 31.27175355779120025 ) ) ;
#2557 = CARTESIAN_POINT ( 'NONE',  ( 68.29446192123552350, 96.82662215664792882, 13.41040346623746515 ) ) ;
#2558 = CARTESIAN_POINT ( 'NONE',  ( 38.67087568172628664, 95.28607559046729136, 36.71405245301004783 ) ) ;
#2559 = CARTESIAN_POINT ( 'NONE',  ( -141.4692556286852891, -156.9891397928654726, 49.65701158161630957 ) ) ;
#2560 = CARTESIAN_POINT ( 'NONE',  ( 38.01140435219952707, 152.9344580088725536, 35.83527830041809636 ) ) ;
#2561 = CARTESIAN_POINT ( 'NONE',  ( 42.21948215057684450, 144.4575765865522783, 39.21067981925355639 ) ) ;
#2562 = DIRECTION ( 'NONE',  ( -0.000000000000000000, -0.000000000000000000, -1.000000000000000000 ) ) ;
#2563 = EDGE_LOOP ( 'NONE', ( #11816, #5747, #14579, #3772 ) ) ;
#2564 = CARTESIAN_POINT ( 'NONE',  ( 41.64333658814960870, 71.77977050742731535, 30.00020018409699318 ) ) ;
#2565 =( BOUNDED_CURVE ( )  B_SPLINE_CURVE ( 2, ( #15957, #870, #10908, #542, #17611, #7605, #14307, #21050, #18156, #13096, #14524, #6258, #16495 ),
 .UNSPECIFIED., .F., .T. ) 
 B_SPLINE_CURVE_WITH_KNOTS ( ( 3, 2, 2, 2, 2, 2, 3 ),
 ( 0.3750000000000000000, 0.3764705882352941124, 0.3794117647058823373, 0.3823529411764705621, 0.3852941176470588425, 0.3882352941176470673, 0.3897058823529411797 ),
 .UNSPECIFIED. ) 
 CURVE ( )  GEOMETRIC_REPRESENTATION_ITEM ( )  RATIONAL_B_SPLINE_CURVE ( ( 0.9755282581475768211, 0.9755282581475768211, 1.000000000000000000, 0.9510565162951535312, 1.000000000000000000, 0.9510565162951535312, 1.000000000000000000, 0.9510565162951535312, 1.000000000000000000, 0.9510565162951535312, 1.000000000000000000, 0.9755282581475768211, 0.9755282581475768211 ) ) 
 REPRESENTATION_ITEM ( '' )  );
#2566 = CARTESIAN_POINT ( 'NONE',  ( -157.2955611005346270, -161.3438272943107563, 41.63779006702063867 ) ) ;
#2567 = CARTESIAN_POINT ( 'NONE',  ( 23.23160898551418185, 147.7622765488190453, -10.85157364460736140 ) ) ;
#2568 = LINE ( 'NONE', #2671, #12905 ) ;
#2569 = ORIENTED_EDGE ( 'NONE', *, *, #16333, .F. ) ;
#2570 = CARTESIAN_POINT ( 'NONE',  ( 43.01140435219951286, 86.03445800887256212, 29.21067981925356705 ) ) ;
#2571 = CARTESIAN_POINT ( 'NONE',  ( 41.64333658814960870, 122.7797705074273296, 30.00020018409699318 ) ) ;
#2572 = ORIENTED_EDGE ( 'NONE', *, *, #9917, .F. ) ;
#2573 = LINE ( 'NONE', #5773, #19594 ) ;
#2574 = VERTEX_POINT ( 'NONE', #13676 ) ;
#2575 = CARTESIAN_POINT ( 'NONE',  ( 41.64333658814960870, 129.9797705074273040, 38.42115945441014446 ) ) ;
#2576 = CARTESIAN_POINT ( 'NONE',  ( 47.05648932407426344, 144.9844580088725934, 37.14960608071593384 ) ) ;
#2577 = ADVANCED_FACE ( 'NONE', ( #20626 ), #13998, .T. ) ;
#2578 = CARTESIAN_POINT ( 'NONE',  ( 39.92123440845005433, 110.3344580088725735, 29.95742577749336988 ) ) ;
#2579 = DIRECTION ( 'NONE',  ( 0.2768218020313508165, -0.9609212714474144601, 0.000000000000000000 ) ) ;
#2580 = CARTESIAN_POINT ( 'NONE',  ( 173.3794444120442506, -136.9891397928655010, -17.64809332337413750 ) ) ;
#2581 = CARTESIAN_POINT ( 'NONE',  ( -141.4692556286852891, -189.9891397928654726, 49.65701158161630957 ) ) ;
#2582 = CARTESIAN_POINT ( 'NONE',  ( 42.21948215057684450, 90.45757658655230671, 39.21067981925355639 ) ) ;
#2583 = CARTESIAN_POINT ( 'NONE',  ( 136.1559806577886036, 182.1353248703794350, 23.62031749096655275 ) ) ;
#2584 = CARTESIAN_POINT ( 'NONE',  ( -154.5594255724347761, -161.1630981290892919, 40.14644641866476604 ) ) ;
#2585 = APPLICATION_PROTOCOL_DEFINITION ( 'draft international standard', 'automotive_design', 1998, #18727 ) ;
#2586 = CARTESIAN_POINT ( 'NONE',  ( 38.01140435219951996, 137.6344580088725991, 32.58608133808903773 ) ) ;
#2587 = CARTESIAN_POINT ( 'NONE',  ( 46.59305225739526435, 104.1797705074273210, 31.60846029578754468 ) ) ;
#2588 = CARTESIAN_POINT ( 'NONE',  ( 29.27693512915957541, 95.18479568265063051, 6.985315079919499404 ) ) ;
#2589 = CARTESIAN_POINT ( 'NONE',  ( -157.2955611005346270, -188.3438272943107279, 41.63779006702063867 ) ) ;
#2590 = CARTESIAN_POINT ( 'NONE',  ( 38.58424406990785371, 93.26518717409400949, 35.64915139335015937 ) ) ;
#2591 = CARTESIAN_POINT ( 'NONE',  ( 43.01140435219951996, 10.71049967264875491, 29.21067981925357060 ) ) ;
#2592 = VERTEX_POINT ( 'NONE', #5201 ) ;
#2593 = CARTESIAN_POINT ( 'NONE',  ( 38.01140435219952707, 87.56049967264873146, 32.58608133808903773 ) ) ;
#2594 = CARTESIAN_POINT ( 'NONE',  ( 11.67247064774405452, 106.1322524520788875, 1.624861436118421043 ) ) ;
#2595 = CARTESIAN_POINT ( 'NONE',  ( 32.21091799184858218, 93.94358800413606048, -12.14875741943239085 ) ) ;
#2596 = CARTESIAN_POINT ( 'NONE',  ( 10.42839491720816625, 130.4056617841633283, -4.565575592310756825 ) ) ;
#2597 = CARTESIAN_POINT ( 'NONE',  ( 40.27526882409969744, 80.92977050742730682, 30.44471234641812174 ) ) ;
#2598 = EDGE_LOOP ( 'NONE', ( #791, #15937, #339, #11454 ) ) ;
#2599 = EDGE_CURVE ( 'NONE', #3989, #14342, #7299, .T. ) ;
#2600 = ORIENTED_EDGE ( 'NONE', *, *, #20829, .T. ) ;
#2601 = CARTESIAN_POINT ( 'NONE',  ( 46.59305225739526435, 157.5797705074273267, 36.81289934271958941 ) ) ;
#2602 = LINE ( 'NONE', #8124, #17554 ) ;
#2603 = AXIS2_PLACEMENT_3D ( 'NONE', #20097, #8623, #20628 ) ;
#2604 = EDGE_CURVE ( 'NONE', #711, #10505, #8246, .T. ) ;
#2605 = CARTESIAN_POINT ( 'NONE',  ( 38.01140435219952707, 117.7104996726487371, 34.21067981925357060 ) ) ;
#2607 = CARTESIAN_POINT ( 'NONE',  ( 27.13677837140323490, 150.1474281128565167, -2.704124018797368301 ) ) ;
#2606 = CARTESIAN_POINT ( 'NONE',  ( 44.37947211624943833, 80.21518717409399812, 30.00020018409699318 ) ) ;
#2608 = CARTESIAN_POINT ( 'NONE',  ( -148.5561028927606344, -170.7938272943107165, 40.69124936498395328 ) ) ;
#2609 = CARTESIAN_POINT ( 'NONE',  ( 43.01140435219954838, 131.9604996726487229, 29.21067981925356705 ) ) ;
#2610 = CARTESIAN_POINT ( 'NONE',  ( -141.4692556286852891, -189.2130981290893317, 52.90620854394536821 ) ) ;
#2611 = DIRECTION ( 'NONE',  ( 1.000000000000000000, 0.000000000000000000, 0.000000000000000000 ) ) ;
#2612 = CARTESIAN_POINT ( 'NONE',  ( 42.21948215057684450, 150.4575765865522783, 39.21067981925356349 ) ) ;
#2613 = CARTESIAN_POINT ( 'NONE',  ( 43.01140435219951286, 146.6297705074273381, 29.55568802177586463 ) ) ;
#2614 = CARTESIAN_POINT ( 'NONE',  ( 13.37233465371036090, 102.6159639102351093, 7.501340520787425525 ) ) ;
#2615 = CARTESIAN_POINT ( 'NONE',  ( 43.01140435219951286, 123.8651871740939896, 38.86567161673127657 ) ) ;
#2616 = SURFACE_SIDE_STYLE ('',( #2512 ) ) ;
#2617 = CARTESIAN_POINT ( 'NONE',  ( -142.0420953463935803, -156.5084106276439968, 46.59394152635518083 ) ) ;
#2618 = CARTESIAN_POINT ( 'NONE',  ( 40.27526882409969033, 59.92977050742730682, 30.44471234641811819 ) ) ;
#2619 = CARTESIAN_POINT ( 'NONE',  ( 109.8528842077358405, 344.7014318495014322, -19.99999999999997868 ) ) ;
#2620 = CARTESIAN_POINT ( 'NONE',  ( 64.30534519084480394, 138.3942263399134447, -9.129458798097310535 ) ) ;
#2621 =( NAMED_UNIT ( * ) PLANE_ANGLE_UNIT ( ) SI_UNIT ( $, .RADIAN. ) );
#2622 = CARTESIAN_POINT ( 'NONE',  ( 47.43856463449117200, 106.4651871740939981, 35.64915139335016647 ) ) ;
#2623 =( BOUNDED_CURVE ( )  B_SPLINE_CURVE ( 2, ( #13699, #6673, #5008, #15366, #5427, #10406, #12046, #13804, #20434, #18453, #258, #16788, #18775 ),
 .UNSPECIFIED., .F., .F. ) 
 B_SPLINE_CURVE_WITH_KNOTS ( ( 3, 2, 2, 2, 2, 2, 3 ),
 ( 0.2867647058823529216, 0.2882352941176470340, 0.2911764705882353144, 0.2941176470588235392, 0.2970588235294117641, 0.2999999999999999889, 0.3014705882352941013 ),
 .UNSPECIFIED. ) 
 CURVE ( )  GEOMETRIC_REPRESENTATION_ITEM ( )  RATIONAL_B_SPLINE_CURVE ( ( 0.9755282581475768211, 0.9755282581475768211, 1.000000000000000000, 0.9510565162951535312, 1.000000000000000000, 0.9510565162951535312, 1.000000000000000000, 0.9510565162951535312, 1.000000000000000000, 0.9510565162951535312, 1.000000000000000000, 0.9755282581475768211, 0.9755282581475768211 ) ) 
 REPRESENTATION_ITEM ( '' )  );
#2624 = ORIENTED_EDGE ( 'NONE', *, *, #6281, .F. ) ;
#2625 = DIRECTION ( 'NONE',  ( 0.000000000000000000, -1.000000000000000000, 0.000000000000000000 ) ) ;
#2626 = VERTEX_POINT ( 'NONE', #13889 ) ;
#2627 = CARTESIAN_POINT ( 'NONE',  ( 48.01140435219951996, 88.28445800887257633, 34.21067981925357060 ) ) ;
#2628 = CARTESIAN_POINT ( 'NONE',  ( 108.9927164799167372, 227.3511983043831037, -5.999999999999976019 ) ) ;
#2629 = CARTESIAN_POINT ( 'NONE',  ( 47.05648932407426344, 152.5104996726487343, 31.27175355779120025 ) ) ;
#2631 = CARTESIAN_POINT ( 'NONE',  ( 65.16383128666855384, 137.2272505635282585, -1.077070130972596962 ) ) ;
#2630 = CARTESIAN_POINT ( 'NONE',  ( 38.58424406990786082, 102.1151871740940180, 34.21067981925357060 ) ) ;
#2632 = CARTESIAN_POINT ( 'NONE',  ( 43.01140435219951286, 65.96049967264873715, 28.95336869806222779 ) ) ;
#2634 = CARTESIAN_POINT ( 'NONE',  ( 43.80332655382220253, 60.61133943119284595, 39.21067981925355639 ) ) ;
#2633 = CARTESIAN_POINT ( 'NONE',  ( 48.01156915178761864, 144.4019414068667686, 34.53828804502998651 ) ) ;
#2635 = FILL_AREA_STYLE ('',( #6156 ) ) ;
#2636 = CARTESIAN_POINT ( 'NONE',  ( -161.4692556286852891, -187.4130981290893203, 52.90620854394536821 ) ) ;
#2637 = LINE ( 'NONE', #1208, #3416 ) ;
#2638 = CARTESIAN_POINT ( 'NONE',  ( 44.37947211624943833, 73.01518717409399528, 38.42115945441014446 ) ) ;
#2639 = DIRECTION ( 'NONE',  ( 0.000000000000000000, 0.000000000000000000, -1.000000000000000000 ) ) ;
#2640 = CARTESIAN_POINT ( 'NONE',  ( 43.01140435219951286, 95.96049967264873715, 29.21067981925356705 ) ) ;
#2641 = VECTOR ( 'NONE', #14185, 1000.000000000000227 ) ;
#2642 = CARTESIAN_POINT ( 'NONE',  ( -148.5561028927606344, -174.9938272943107336, 58.62277379824867296 ) ) ;
#2643 = CARTESIAN_POINT ( 'NONE',  ( -160.8964159109769696, -185.3084106276440366, 46.59394152635518083 ) ) ;
#2644 = ORIENTED_EDGE ( 'NONE', *, *, #20541, .F. ) ;
#2645 = CARTESIAN_POINT ( 'NONE',  ( -145.6429501568359797, -169.1084106276440480, 57.67623309621198047 ) ) ;
#2646 = CARTESIAN_POINT ( 'NONE',  ( 32.75162935850930523, 152.6515011162663313, 2.501635869428501469 ) ) ;
#2647 = CARTESIAN_POINT ( 'NONE',  ( 144.5586921005913439, 133.1239846058259388, -25.00000000000000000 ) ) ;
#2648 = CARTESIAN_POINT ( 'NONE',  ( 44.37947211624943833, 139.0151871740939953, 38.42115945441014446 ) ) ;
#2649 = CARTESIAN_POINT ( 'NONE',  ( 39.42975644700377558, 93.07977050742731251, 31.60846029578754468 ) ) ;
#2650 = ORIENTED_EDGE ( 'NONE', *, *, #6268, .T. ) ;
#2651 = EDGE_LOOP ( 'NONE', ( #10950, #13324, #7415, #10977 ) ) ;
#2652 = CARTESIAN_POINT ( 'NONE',  ( 58.92189266798492042, 143.1894642327317513, 11.58510527907202992 ) ) ;
#2653 = ORIENTED_EDGE ( 'NONE', *, *, #14566, .F. ) ;
#2654 = CARTESIAN_POINT ( 'NONE',  ( 46.10157429594899270, 112.7344580088725792, 29.95742577749337343 ) ) ;
#2655 = CARTESIAN_POINT ( 'NONE',  ( 43.01140435219951996, 10.71049967264875491, 34.21067981925357060 ) ) ;
#2656 = CARTESIAN_POINT ( 'NONE',  ( 39.42975644700377558, 81.07977050742731251, 31.60846029578754468 ) ) ;
#2657 = CARTESIAN_POINT ( 'NONE',  ( 41.64333658814960870, 138.7151871740940123, 38.42115945441014446 ) ) ;
#2658 = CARTESIAN_POINT ( 'NONE',  ( 48.01140435219951996, 89.06049967264871725, 35.83527830041810347 ) ) ;
#2659 = CARTESIAN_POINT ( 'NONE',  ( 69.83118287335672392, 141.1824132108841638, 4.838974892866481525 ) ) ;
#2660 = CARTESIAN_POINT ( 'NONE',  ( 41.70806931348493407, 94.93898644073527748, 39.04902473919937478 ) ) ;
#2661 = CARTESIAN_POINT ( 'NONE',  ( -161.4692556286852607, -164.3391397928654385, 52.90620854394536821 ) ) ;
#2662 = CARTESIAN_POINT ( 'NONE',  ( -149.8854112254399240, -158.3899795514095672, 39.65701158161629536 ) ) ;
#2663 = UNCERTAINTY_MEASURE_WITH_UNIT (LENGTH_MEASURE( 1.000000000000000082E-05 ), #12101, 'distance_accuracy_value', 'NONE');
#2664 = EDGE_CURVE ( 'NONE', #10827, #15137, #5819, .T. ) ;
#2665 = CARTESIAN_POINT ( 'NONE',  ( 47.05648932407426344, 106.9104996726487400, 37.14960608071593384 ) ) ;
#2666 = DIRECTION ( 'NONE',  ( 0.000000000000000000, 1.000000000000000000, 0.000000000000000000 ) ) ;
#2667 = ORIENTED_EDGE ( 'NONE', *, *, #5537, .T. ) ;
#2668 = CARTESIAN_POINT ( 'NONE',  ( 40.27526882409969033, 72.82977050742732672, 37.97664729208901946 ) ) ;
#2669 = CARTESIAN_POINT ( 'NONE',  ( -142.0420953463936087, -165.3938272943107393, 49.65701158161630957 ) ) ;
#2670 = CARTESIAN_POINT ( 'NONE',  ( 74.62708615766334219, 133.0342049366344384, -8.851289726714327344 ) ) ;
#2671 = CARTESIAN_POINT ( 'NONE',  ( -138.5468111011521160, 759.4679229819337252, -0.8325491102011938205 ) ) ;
#2672 = AXIS2_PLACEMENT_3D ( 'NONE', #18216, #12932, #19656 ) ;
#2673 = EDGE_LOOP ( 'NONE', ( #7016, #20805 ) ) ;
#2674 = CARTESIAN_POINT ( 'NONE',  ( 147.5268905834513475, 193.0332408774651185, -44.99999999999997158 ) ) ;
#2675 = CIRCLE ( 'NONE', #7981, 10.00000000000000888 ) ;
#2676 = CARTESIAN_POINT ( 'NONE',  ( 43.01140435219951286, 123.5344580088725621, 39.21067981925356349 ) ) ;
#2677 = CARTESIAN_POINT ( 'NONE',  ( 46.59305225739526435, 125.1797705074273210, 31.60846029578754468 ) ) ;
#2678 = ORIENTED_EDGE ( 'NONE', *, *, #16774, .T. ) ;
#2679 = CARTESIAN_POINT ( 'NONE',  ( 43.01140435219951996, 10.71049967264875491, 34.21067981925357060 ) ) ;
#2680 = VERTEX_POINT ( 'NONE', #15549 ) ;
#2681 = CARTESIAN_POINT ( 'NONE',  ( 47.43856463449117200, 122.0297705074273011, 32.77220824515698183 ) ) ;
#2682 = EDGE_CURVE ( 'NONE', #13485, #15661, #214, .T. ) ;
#2683 = CARTESIAN_POINT ( 'NONE',  ( 43.80332655382220253, 144.6113394311928744, 39.21067981925355639 ) ) ;
#2684 = CARTESIAN_POINT ( 'NONE',  ( 38.01140435219951996, 59.63445800887255643, 32.58608133808903773 ) ) ;
#2685 = VECTOR ( 'NONE', #15626, 1000.000000000000000 ) ;
#2686 = CARTESIAN_POINT ( 'NONE',  ( 84.42064422693164261, 282.0082918409407284, 4.000000000000003553 ) ) ;
#2687 = DIRECTION ( 'NONE',  ( 0.3450121214752276400, -0.9385982292947087080, 0.000000000000000000 ) ) ;
#2688 = CARTESIAN_POINT ( 'NONE',  ( 151.4773229304660731, 84.89323405393692212, 14.00000000000001776 ) ) ;
#2689 = STYLED_ITEM ( 'NONE', ( #6670 ), #14549 ) ;
#2690 = CARTESIAN_POINT ( 'NONE',  ( -143.3790856849358306, -190.2891397928654555, 55.53486410454105027 ) ) ;
#2691 =( BOUNDED_CURVE ( )  B_SPLINE_CURVE ( 2, ( #13190, #4587, #14832, #4811, #12973, #19699, #18261, #6588, #13307, #11307, #3164, #18034, #9678 ),
 .UNSPECIFIED., .F., .F. ) 
 B_SPLINE_CURVE_WITH_KNOTS ( ( 3, 2, 2, 2, 2, 2, 3 ),
 ( 0.6964285714285713969, 0.6999999999999999556, 0.7071428571428571841, 0.7142857142857143016, 0.7214285714285714191, 0.7285714285714285365, 0.7321428571428572063 ),
 .UNSPECIFIED. ) 
 CURVE ( )  GEOMETRIC_REPRESENTATION_ITEM ( )  RATIONAL_B_SPLINE_CURVE ( ( 0.9755282581475768211, 0.9755282581475768211, 1.000000000000000000, 0.9510565162951535312, 1.000000000000000000, 0.9510565162951535312, 1.000000000000000000, 0.9510565162951535312, 1.000000000000000000, 0.9510565162951535312, 1.000000000000000000, 0.9755282581475763770, 0.9755282581475768211 ) ) 
 REPRESENTATION_ITEM ( '' )  );
#2692 = CARTESIAN_POINT ( 'NONE',  ( 39.92123440845005433, 66.26049967264874851, 29.95742577749336988 ) ) ;
#2693 = LINE ( 'NONE', #7565, #6529 ) ;
#2694 = CARTESIAN_POINT ( 'NONE',  ( -151.4692556286852891, -188.6438272943107393, 39.74470866294723947 ) ) ;
#2695 = PRODUCT_CONTEXT ( 'NONE', #5614, 'mechanical' ) ;
#2696 = CARTESIAN_POINT ( 'NONE',  ( 43.01140435219951286, 134.0344580088726048, 28.95336869806222779 ) ) ;
#2697 = CARTESIAN_POINT ( 'NONE',  ( 38.58424406990784661, 108.5297705074273011, 35.64915139335016647 ) ) ;
#2698 = CARTESIAN_POINT ( 'NONE',  ( 62.38482844916680392, 99.30468409114129713, 12.58043553469319953 ) ) ;
#2699 = CARTESIAN_POINT ( 'NONE',  ( -151.4692556286852891, -191.6438272943107108, 39.74470866294723947 ) ) ;
#2700 = CARTESIAN_POINT ( 'NONE',  ( 38.58424406990785371, 102.2651871740939811, 35.64915139335015937 ) ) ;
#2701 = CARTESIAN_POINT ( 'NONE',  ( 43.01140435219951996, 119.9070776186055838, -35.00000000000000000 ) ) ;
#2702 = ORIENTED_EDGE ( 'NONE', *, *, #5054, .F. ) ;
#2703 = DIRECTION ( 'NONE',  ( -0.000000000000000000, -0.000000000000000000, 1.000000000000000000 ) ) ;
#2704 = ADVANCED_FACE ( 'NONE', ( #6860 ), #10706, .T. ) ;
#2705 = CARTESIAN_POINT ( 'NONE',  ( 25.52397925108762067, 90.47728371212039633, 7.934596195134201224 ) ) ;
#2706 = CARTESIAN_POINT ( 'NONE',  ( 45.74753988029934249, 146.3297705074273267, 30.44471234641812174 ) ) ;
#2707 = CARTESIAN_POINT ( 'NONE',  ( 52.12662541604375122, 146.5080492276505311, -15.72009227599853531 ) ) ;
#2708 = PRODUCT_DEFINITION_SHAPE ( 'NONE', 'NONE',  #21824 ) ;
#2709 = CARTESIAN_POINT ( 'NONE',  ( 32.98198692859195802, 152.6383102900375093, -3.493975233523312962 ) ) ;
#2710 = CARTESIAN_POINT ( 'NONE',  ( 47.43856463449117911, 76.72977050742731819, 35.64915139335015937 ) ) ;
#2711 = ORIENTED_EDGE ( 'NONE', *, *, #8181, .F. ) ;
#2712 = ORIENTED_EDGE ( 'NONE', *, *, #19599, .F. ) ;
#2713 = CARTESIAN_POINT ( 'NONE',  ( 40.27526882409969033, 153.8297705074273267, 37.97664729208901946 ) ) ;
#2714 = CARTESIAN_POINT ( 'NONE',  ( -151.4692556286852891, -196.9891397928655010, 49.65701158161630957 ) ) ;
#2715 = AXIS2_PLACEMENT_3D ( 'NONE', #9298, #2346, #696 ) ;
#2716 = CARTESIAN_POINT ( 'NONE',  ( 43.01140435219951286, 119.9604996726487229, 28.95336869806222779 ) ) ;
#2718 = CARTESIAN_POINT ( 'NONE',  ( 17.52322149637394233, 97.17389352242535949, -4.727774211004094340 ) ) ;
#2717 = CARTESIAN_POINT ( 'NONE',  ( 41.64333658814960870, 77.51518717409399528, 30.00020018409699318 ) ) ;
#2719 = CARTESIAN_POINT ( 'NONE',  ( 116.9721770337685882, 160.7104996726487514, -35.00000000000000000 ) ) ;
#2720 = CARTESIAN_POINT ( 'NONE',  ( -142.0420953463936087, -171.3938272943107393, 49.65701158161630957 ) ) ;
#2721 = AXIS2_PLACEMENT_3D ( 'NONE', #1022, #14760, #2452 ) ;
#2722 = CARTESIAN_POINT ( 'NONE',  ( 24.41145734808947054, 148.6458414325078081, 10.19629000755267434 ) ) ;
#2723 = CARTESIAN_POINT ( 'NONE',  ( -145.2889157411863721, -189.5130981290893146, 58.16351966513671812 ) ) ;
#2724 =( LENGTH_UNIT ( ) NAMED_UNIT ( * ) SI_UNIT ( .MILLI., .METRE. ) );
#2725 = DIRECTION ( 'NONE',  ( -0.000000000000000000, -0.000000000000000000, -1.000000000000000000 ) ) ;
#2726 = CARTESIAN_POINT ( 'NONE',  ( 42.21948215057684450, 149.1113394311928744, 29.21067981925357060 ) ) ;
#2727 = CARTESIAN_POINT ( 'NONE',  ( 47.43856463449118621, 133.8797705074273381, 34.21067981925357060 ) ) ;
#2728 = EDGE_CURVE ( 'NONE', #14631, #14663, #15698, .T. ) ;
#2729 = CARTESIAN_POINT ( 'NONE',  ( 66.97354912532109950, 95.34500505098478129, 5.477698430975745048 ) ) ;
#2730 = CARTESIAN_POINT ( 'NONE',  ( 44.37947211624943833, 128.2151871740939839, 30.00020018409699318 ) ) ;
#2731 = DIRECTION ( 'NONE',  ( 0.000000000000000000, 0.000000000000000000, 1.000000000000000000 ) ) ;
#2732 = CARTESIAN_POINT ( 'NONE',  ( 38.01140435219952707, 150.5604996726487457, 32.58608133808903773 ) ) ;
#2733 = DIRECTION ( 'NONE',  ( 0.9949940778855791423, 0.09993390301907582873, 0.000000000000000000 ) ) ;
#2734 = DIRECTION ( 'NONE',  ( -0.000000000000000000, -0.000000000000000000, -1.000000000000000000 ) ) ;
#2735 = CARTESIAN_POINT ( 'NONE',  ( 32.03768905382736421, 145.5187656067679711, 23.43402463578956585 ) ) ;
#2736 = AXIS2_PLACEMENT_3D ( 'NONE', #20692, #841, #10665 ) ;
#2737 = CARTESIAN_POINT ( 'NONE',  ( -47.86331837773882825, -37.13255853780189852, -25.00000000000000000 ) ) ;
#2738 = CARTESIAN_POINT ( 'NONE',  ( 43.01140435219951286, 110.3651871740939754, 29.55568802177586463 ) ) ;
#2739 = ORIENTED_EDGE ( 'NONE', *, *, #19264, .T. ) ;
#2740 = VECTOR ( 'NONE', #14647, 1000.000000000000000 ) ;
#2741 = CARTESIAN_POINT ( 'NONE',  ( 48.01140435219951996, 86.21049967264873715, 34.21067981925357060 ) ) ;
#2742 = VERTEX_POINT ( 'NONE', #3765 ) ;
#2743 = CARTESIAN_POINT ( 'NONE',  ( 43.01140435219951286, 92.03445800887256212, 28.95336869806222779 ) ) ;
#2744 = DIRECTION ( 'NONE',  ( 0.000000000000000000, 0.000000000000000000, 1.000000000000000000 ) ) ;
#2745 = CARTESIAN_POINT ( 'NONE',  ( 46.10157429594899270, 146.6604996726487400, 29.95742577749337343 ) ) ;
#2747 = CARTESIAN_POINT ( 'NONE',  ( 26.96882349746146446, 96.81297435472995971, -11.91061488385382106 ) ) ;
#2746 = CARTESIAN_POINT ( 'NONE',  ( 39.42975644700377558, 107.8151871740939924, 31.60846029578754468 ) ) ;
#2748 = CARTESIAN_POINT ( 'NONE',  ( 26.17254549292281141, -61.68114226949890622, 20.00000000000000355 ) ) ;
#2749 = DIRECTION ( 'NONE',  ( 0.000000000000000000, 1.000000000000000000, 0.000000000000000000 ) ) ;
#2750 = FACE_OUTER_BOUND ( 'NONE', #21346, .T. ) ;
#2751 = CARTESIAN_POINT ( 'NONE',  ( 44.55648932407425633, 79.88445800887257064, 29.45539723777780239 ) ) ;
#2752 = CARTESIAN_POINT ( 'NONE',  ( 151.4773229304660731, 84.89323405393692212, 14.00000000000001776 ) ) ;
#2753 = CARTESIAN_POINT ( 'NONE',  ( 43.01140435219951286, 65.36518717409400381, 29.55568802177586463 ) ) ;
#2754 = EDGE_CURVE ( 'NONE', #17127, #13513, #13456, .T. ) ;
#2755 = CARTESIAN_POINT ( 'NONE',  ( 20.91437931538276374, 145.9617080342048894, -10.94665030085253044 ) ) ;
#2756 = CARTESIAN_POINT ( 'NONE',  ( 38.01140435219952707, 114.8604996726487428, 35.83527830041809636 ) ) ;
#2757 = CARTESIAN_POINT ( 'NONE',  ( -143.8425227516148084, -174.6938272943107506, 55.19815736654470584 ) ) ;
#2758 = CARTESIAN_POINT ( 'NONE',  ( -160.8964159109769696, -188.3084106276440650, 46.59394152635518083 ) ) ;
#2759 = ORIENTED_EDGE ( 'NONE', *, *, #9496, .T. ) ;
#2760 = CARTESIAN_POINT ( 'NONE',  ( 44.37947211624943833, 70.01518717409399528, 38.42115945441014446 ) ) ;
#2761 =( BOUNDED_CURVE ( )  B_SPLINE_CURVE ( 2, ( #7654, #9193, #15679, #6389, #15890, #2560, #14027, #14240, #2345, #5975, #19213, #3902, #20760 ),
 .UNSPECIFIED., .F., .F. ) 
 B_SPLINE_CURVE_WITH_KNOTS ( ( 3, 2, 2, 2, 2, 2, 3 ),
 ( 0.05147058823529412214, 0.05294117647058823456, 0.05588235294117647328, 0.05882352941176470507, 0.06176470588235294379, 0.06470588235294118251, 0.06617647058823529493 ),
 .UNSPECIFIED. ) 
 CURVE ( )  GEOMETRIC_REPRESENTATION_ITEM ( )  RATIONAL_B_SPLINE_CURVE ( ( 0.9755282581475768211, 0.9755282581475768211, 1.000000000000000000, 0.9510565162951535312, 1.000000000000000000, 0.9510565162951535312, 1.000000000000000000, 0.9510565162951535312, 1.000000000000000000, 0.9510565162951535312, 1.000000000000000000, 0.9755282581475768211, 0.9755282581475768211 ) ) 
 REPRESENTATION_ITEM ( '' )  );
#2762 = CARTESIAN_POINT ( 'NONE',  ( -145.6429501568359797, -174.2084106276440423, 41.63779006702063867 ) ) ;
#2763 = CARTESIAN_POINT ( 'NONE',  ( 59.95958160670890180, 90.07020311440788873, 19.76341270931769500 ) ) ;
#2764 = CARTESIAN_POINT ( 'NONE',  ( 48.01140435219951996, 112.1344580088725706, 35.83527830041809636 ) ) ;
#2765 = CARTESIAN_POINT ( 'NONE',  ( 40.27526882409969033, 132.5651871740940067, 37.97664729208901946 ) ) ;
#2766 = CARTESIAN_POINT ( 'NONE',  ( 44.37947211624943833, 154.0151871740940237, 38.42115945441014446 ) ) ;
#2767 = EDGE_CURVE ( 'NONE', #6804, #8, #21056, .T. ) ;
#2768 = VERTEX_POINT ( 'NONE', #5833 ) ;
#2769 = ORIENTED_EDGE ( 'NONE', *, *, #21718, .F. ) ;
#2770 = SURFACE_SIDE_STYLE ('',( #17858 ) ) ;
#2771 = ORIENTED_EDGE ( 'NONE', *, *, #19995, .T. ) ;
#2772 = CARTESIAN_POINT ( 'NONE',  ( 43.01140435219951286, 59.96049967264874425, 29.21067981925356705 ) ) ;
#2773 = EDGE_CURVE ( 'NONE', #12910, #3828, #2316, .T. ) ;
#2774 = ADVANCED_FACE ( 'NONE', ( #4505 ), #14211, .F. ) ;
#2775 = CARTESIAN_POINT ( 'NONE',  ( 39.42975644700377558, 72.07977050742732672, 31.60846029578754468 ) ) ;
#2776 = CARTESIAN_POINT ( 'NONE',  ( 41.64333658814960870, 137.5151871740939953, 30.00020018409699318 ) ) ;
#2777 = CARTESIAN_POINT ( 'NONE',  ( 43.01140435219951286, 88.46049967264873715, 39.46799094044489209 ) ) ;
#2778 = CARTESIAN_POINT ( 'NONE',  ( 52.46025766099742071, 152.8098426157893925, 11.14871012209260748 ) ) ;
#2779 = LINE ( 'NONE', #21415, #3675 ) ;
#2780 = CARTESIAN_POINT ( 'NONE',  ( -161.4692556286852607, -161.3391397928654669, 52.90620854394536821 ) ) ;
#2781 = CARTESIAN_POINT ( 'NONE',  ( 43.80332655382220253, 107.8836182503284675, 29.21067981925356705 ) ) ;
#2782 = ORIENTED_EDGE ( 'NONE', *, *, #11167, .F. ) ;
#2783 = CARTESIAN_POINT ( 'NONE',  ( 39.42975644700377558, 72.07977050742732672, 31.60846029578754468 ) ) ;
#2784 = CARTESIAN_POINT ( 'NONE',  ( -155.3247660971250923, -155.4453047235116969, 40.99743995317548695 ) ) ;
#2785 = CARTESIAN_POINT ( 'NONE',  ( 10.91571581598819662, 131.8149664739095783, 9.482090752819161139 ) ) ;
#2786 = AXIS2_PLACEMENT_3D ( 'NONE', #13218, #4841, #6619 ) ;
#2787 = CARTESIAN_POINT ( 'NONE',  ( -143.8425227516148084, -189.9584106276440423, 55.19815736654470584 ) ) ;
#2788 = ORIENTED_EDGE ( 'NONE', *, *, #16877, .F. ) ;
#2789 = FACE_OUTER_BOUND ( 'NONE', #6009, .T. ) ;
#2790 = VECTOR ( 'NONE', #8913, 1000.000000000000000 ) ;
#2791 = CARTESIAN_POINT ( 'NONE',  ( -156.1828684652451784, -155.6591478762521206, 41.49287016839741682 ) ) ;
#2792 = CARTESIAN_POINT ( 'NONE',  ( 43.01140435219951286, 124.1297705074273097, 38.86567161673127657 ) ) ;
#2793 = ORIENTED_EDGE ( 'NONE', *, *, #13155, .T. ) ;
#2794 = CARTESIAN_POINT ( 'NONE',  ( 121.4021762516569964, 137.5714195593754710, 272.0939500981630204 ) ) ;
#2795 = VERTEX_POINT ( 'NONE', #10919 ) ;
#2796 = CARTESIAN_POINT ( 'NONE',  ( 40.27526882409969033, 128.9297705074272926, 30.44471234641811819 ) ) ;
#2797 = CARTESIAN_POINT ( 'NONE',  ( -136.6255475934131596, 760.1741454933652449, -19.99999999999996092 ) ) ;
#2798 = EDGE_CURVE ( 'NONE', #12363, #19770, #19292, .T. ) ;
#2799 = CARTESIAN_POINT ( 'NONE',  ( 38.96631938032478359, 62.48445800887257917, 31.27175355779120025 ) ) ;
#2800 = VECTOR ( 'NONE', #6103, 1000.000000000000000 ) ;
#2801 = CARTESIAN_POINT ( 'NONE',  ( 43.01140435219950575, 139.4604996726487514, 39.21067981925356349 ) ) ;
#2802 = CARTESIAN_POINT ( 'NONE',  ( 38.01140435219952707, 101.7844580088725905, 34.21067981925357060 ) ) ;
#2803 = CARTESIAN_POINT ( 'NONE',  ( -159.5594255724347761, -176.7891397928654840, 43.77915905869157598 ) ) ;
#2804 = CARTESIAN_POINT ( 'NONE',  ( -161.4692556286852607, -188.3391397928654953, 52.90620854394536821 ) ) ;
#2805 = CARTESIAN_POINT ( 'NONE',  ( 41.46631938032478359, 66.11049967264874283, 29.45539723777780239 ) ) ;
#2806 = DIRECTION ( 'NONE',  ( -0.000000000000000000, -0.000000000000000000, -1.000000000000000000 ) ) ;
#2807 = CARTESIAN_POINT ( 'NONE',  ( -142.0420953463935803, -195.2438272943107336, 46.59394152635518793 ) ) ;
#2808 = APPLICATION_PROTOCOL_DEFINITION ( 'draft international standard', 'automotive_design', 1998, #15354 ) ;
#2809 = CARTESIAN_POINT ( 'NONE',  ( 46.10157429594899270, 126.8344580088725451, 38.46393386101376421 ) ) ;
#2810 = CARTESIAN_POINT ( 'NONE',  ( 45.74753988029933538, 100.4297705074273210, 37.97664729208901946 ) ) ;
#2811 = CARTESIAN_POINT ( 'NONE',  ( 35.68099593698222094, 147.2217917141817907, 16.62841781073025871 ) ) ;
#2812 = CARTESIAN_POINT ( 'NONE',  ( -148.5561028927606344, -186.9938272943107336, 58.62277379824867296 ) ) ;
#2813 = CARTESIAN_POINT ( 'NONE',  ( 41.64333658814960870, 101.5151871740939953, 30.00020018409699318 ) ) ;
#2814 = LINE ( 'NONE', #14493, #10358 ) ;
#2815 = VERTEX_POINT ( 'NONE', #15864 ) ;
#2816 = CARTESIAN_POINT ( 'NONE',  ( 44.55648932407425633, 127.6104996726487570, 38.96596240072933170 ) ) ;
#2817 = CARTESIAN_POINT ( 'NONE',  ( 8.927628897234525240, 116.7075971571176751, 1.981832035706394546 ) ) ;
#2818 = CARTESIAN_POINT ( 'NONE',  ( 26.92635752117756098, 142.9018661569831750, -16.76761354414967542 ) ) ;
#2819 = CARTESIAN_POINT ( 'NONE',  ( 47.43856463449117911, 68.02977050742731535, 32.77220824515697473 ) ) ;
#2820 = EDGE_LOOP ( 'NONE', ( #17336, #13853, #8094, #3101 ) ) ;
#2821 = EDGE_LOOP ( 'NONE', ( #1120, #8396, #2909, #14667 ) ) ;
#2822 = CARTESIAN_POINT ( 'NONE',  ( 46.59305225739526435, 155.1797705074273210, 31.60846029578754468 ) ) ;
#2823 = EDGE_CURVE ( 'NONE', #12361, #3465, #12741, .T. ) ;
#2824 = CARTESIAN_POINT ( 'NONE',  ( 44.55648932407425633, 112.6104996726487428, 38.96596240072933170 ) ) ;
#2825 = CARTESIAN_POINT ( 'NONE',  ( 23.23160898551418185, 147.7622765488190453, -10.85157364460736140 ) ) ;
#2826 = CARTESIAN_POINT ( 'NONE',  ( 38.01140435219952707, 95.78445800887259054, 34.21067981925357060 ) ) ;
#2827 = CARTESIAN_POINT ( 'NONE',  ( -145.6429501568359797, -173.9438272943107222, 41.63779006702063867 ) ) ;
#2828 = DIRECTION ( 'NONE',  ( 1.000000000000000000, 0.000000000000000000, 0.000000000000000000 ) ) ;
#2829 = CARTESIAN_POINT ( 'NONE',  ( -159.5594255724347761, -181.8630981290893374, 43.77915905869157598 ) ) ;
#2830 =( NAMED_UNIT ( * ) PLANE_ANGLE_UNIT ( ) SI_UNIT ( $, .RADIAN. ) );
#2831 = DIRECTION ( 'NONE',  ( 1.000000000000000000, 0.000000000000000000, -1.723963091245776585E-16 ) ) ;
#2832 = CARTESIAN_POINT ( 'NONE',  ( 38.01140435219952707, 149.7844580088725763, 34.21067981925357060 ) ) ;
#2833 = CARTESIAN_POINT ( 'NONE',  ( 40.27526882409969033, 128.9297705074272926, 30.44471234641811819 ) ) ;
#2834 = CARTESIAN_POINT ( 'NONE',  ( 55.35048440753327981, 87.88826800209452017, -1.070088050731120344 ) ) ;
#2835 = CARTESIAN_POINT ( 'NONE',  ( 41.64333658814960870, 129.7151871740940123, 38.42115945441014446 ) ) ;
#2836 = FILL_AREA_STYLE_COLOUR ( '', #20940 ) ;
#2837 = CARTESIAN_POINT ( 'NONE',  ( -120.0322075325610740, -126.9891397928655010, 49.65701158161630957 ) ) ;
#2838 = CARTESIAN_POINT ( 'NONE',  ( 173.3794444120442506, -126.9891397928655010, 19.99999999999999645 ) ) ;
#2839 = LINE ( 'NONE', #9580, #85 ) ;
#2840 = CARTESIAN_POINT ( 'NONE',  ( 71.17671054099098171, 117.3556635612232810, 18.77100214853170357 ) ) ;
#2841 = CARTESIAN_POINT ( 'NONE',  ( 116.9721770337685740, 133.1239846058259388, -25.00000000000000000 ) ) ;
#2842 = ORIENTED_EDGE ( 'NONE', *, *, #14486, .F. ) ;
#2843 = LINE ( 'NONE', #18047, #84 ) ;
#2844 = ORIENTED_EDGE ( 'NONE', *, *, #8212, .T. ) ;
#2845 = CARTESIAN_POINT ( 'NONE',  ( 44.55648932407425633, 81.68445800887258201, 38.96596240072933170 ) ) ;
#2846 = DIRECTION ( 'NONE',  ( -0.000000000000000000, -0.000000000000000000, 1.000000000000000000 ) ) ;
#2847 = CARTESIAN_POINT ( 'NONE',  ( 47.05648932407426344, 145.9104996726487400, 37.14960608071593384 ) ) ;
#2849 = CARTESIAN_POINT ( 'NONE',  ( 56.57648482392179545, 95.27494636639178793, 7.851242587554376762 ) ) ;
#2848 = CARTESIAN_POINT ( 'NONE',  ( 46.59305225739526435, 100.9151871740940010, 31.60846029578754468 ) ) ;
#2850 = EDGE_CURVE ( 'NONE', #11358, #11797, #16663, .T. ) ;
#2851 = CARTESIAN_POINT ( 'NONE',  ( -148.5561028927606344, -169.2584106276440536, 58.62277379824867296 ) ) ;
#2852 = CARTESIAN_POINT ( 'NONE',  ( 44.55648932407425633, 64.61049967264874283, 38.96596240072933170 ) ) ;
#2854 = CARTESIAN_POINT ( 'NONE',  ( -149.8854112254399240, -183.7362167067689995, 59.65701158161632378 ) ) ;
#2853 = DIRECTION ( 'NONE',  ( -0.000000000000000000, -0.000000000000000000, 1.000000000000000000 ) ) ;
#2855 = CARTESIAN_POINT ( 'NONE',  ( -145.2889157411863437, -189.5130981290893146, 58.16351966513671812 ) ) ;
#2856 = DIRECTION ( 'NONE',  ( 1.000000000000000000, -0.000000000000000000, -0.000000000000000000 ) ) ;
#2857 = PLANE ( 'NONE',  #8341 ) ;
#2858 = CARTESIAN_POINT ( 'NONE',  ( 41.64333658814960870, 63.71518717409399812, 38.42115945441014446 ) ) ;
#2859 = CARTESIAN_POINT ( 'NONE',  ( 69.71972837475884432, 98.49221204361529658, -7.660766391518695428 ) ) ;
#2860 = CARTESIAN_POINT ( 'NONE',  ( 43.01140435219951286, 150.8651871740939896, 38.86567161673127657 ) ) ;
#2861 = LINE ( 'NONE', #6061, #16612 ) ;
#2862 = CARTESIAN_POINT ( 'NONE',  ( -157.2955611005346270, -170.3438272943107563, 41.63779006702063867 ) ) ;
#2863 = CARTESIAN_POINT ( 'NONE',  ( -143.8425227516148084, -180.3584106276440480, 44.11586579668791330 ) ) ;
#2864 = EDGE_LOOP ( 'NONE', ( #515, #9206, #2842, #9559 ) ) ;
#2865 = CARTESIAN_POINT ( 'NONE',  ( 43.01140435219951286, 71.36518717409398960, 29.55568802177586107 ) ) ;
#2866 = CARTESIAN_POINT ( 'NONE',  ( -142.0420953463936087, -165.6584106276440593, 49.65701158161630957 ) ) ;
#2867 = CARTESIAN_POINT ( 'NONE',  ( 74.43934690056714487, 106.1333445020626129, 19.04903893889577660 ) ) ;
#2868 = LINE ( 'NONE', #18073, #21489 ) ;
#2869 = CARTESIAN_POINT ( 'NONE',  ( 47.43856463449117200, 130.7651871740939953, 32.77220824515698183 ) ) ;
#2870 = ADVANCED_FACE ( 'NONE', ( #991 ), #14430, .T. ) ;
#2871 = CARTESIAN_POINT ( 'NONE',  ( 77.09984031027478579, 117.8059907461747429, -7.347010041119995449 ) ) ;
#2872 = ORIENTED_EDGE ( 'NONE', *, *, #5164, .F. ) ;
#2873 = ORIENTED_EDGE ( 'NONE', *, *, #19692, .F. ) ;
#2874 = VECTOR ( 'NONE', #16221, 1000.000000000000000 ) ;
#2875 = ADVANCED_FACE ( 'NONE', ( #11445 ), #11665, .F. ) ;
#2876 = CIRCLE ( 'NONE', #14842, 9.999999999999994671 ) ;
#2877 = ORIENTED_EDGE ( 'NONE', *, *, #6972, .T. ) ;
#2878 = ADVANCED_FACE ( 'NONE', ( #1205 ), #16736, .T. ) ;
#2879 = DIRECTION ( 'NONE',  ( 0.000000000000000000, 1.000000000000000000, 0.000000000000000000 ) ) ;
#2880 = CIRCLE ( 'NONE', #15211, 10.00000000000000888 ) ;
#2881 = CARTESIAN_POINT ( 'NONE',  ( 47.43856463449117200, 77.02977050742731535, 32.77220824515698183 ) ) ;
#2883 = CARTESIAN_POINT ( 'NONE',  ( 27.67177345608778793, 143.5689829720894011, 10.27550654291302479 ) ) ;
#2882 = CARTESIAN_POINT ( 'NONE',  ( 38.58424406990786082, 138.1151871740940180, 34.21067981925357060 ) ) ;
#2884 = EDGE_CURVE ( 'NONE', #5761, #1030, #19493, .T. ) ;
#2885 = CARTESIAN_POINT ( 'NONE',  ( 43.01140435219951286, 92.96049967264873715, 28.95336869806222779 ) ) ;
#2886 = CARTESIAN_POINT ( 'NONE',  ( 51.78234217841457365, 152.9971814535558963, 4.124977536042813142 ) ) ;
#2887 = PLANE ( 'NONE',  #7204 ) ;
#2888 = CARTESIAN_POINT ( 'NONE',  ( -143.3790856849358306, -163.2891397928654555, 55.53486410454105027 ) ) ;
#2889 =( BOUNDED_CURVE ( )  B_SPLINE_CURVE ( 2, ( #14252, #924, #3811, #20996, #15591, #20885, #20672, #5556, #12280, #4233, #15906, #817, #13933 ),
 .UNSPECIFIED., .F., .F. ) 
 B_SPLINE_CURVE_WITH_KNOTS ( ( 3, 2, 2, 2, 2, 2, 3 ),
 ( 0.8308823529411765163, 0.8323529411764706287, 0.8352941176470588536, 0.8382352941176470784, 0.8411764705882353033, 0.8441176470588235281, 0.8455882352941176405 ),
 .UNSPECIFIED. ) 
 CURVE ( )  GEOMETRIC_REPRESENTATION_ITEM ( )  RATIONAL_B_SPLINE_CURVE ( ( 0.9755282581475768211, 0.9755282581475768211, 1.000000000000000000, 0.9510565162951535312, 1.000000000000000000, 0.9510565162951535312, 1.000000000000000000, 0.9510565162951535312, 1.000000000000000000, 0.9510565162951535312, 1.000000000000000000, 0.9755282581475768211, 0.9755282581475768211 ) ) 
 REPRESENTATION_ITEM ( '' )  );
#2890 = CARTESIAN_POINT ( 'NONE',  ( 41.64333658814960870, 83.51518717409400949, 30.00020018409699318 ) ) ;
#2891 = DIRECTION ( 'NONE',  ( -0.3450121214752278065, 0.9385982292947087080, -0.000000000000000000 ) ) ;
#2892 = PRODUCT_DEFINITION_SHAPE ( 'NONE', 'NONE',  #21830 ) ;
#2893 = AXIS2_PLACEMENT_3D ( 'NONE', #7958, #11580, #15332 ) ;
#2894 = CARTESIAN_POINT ( 'NONE',  ( 43.01140435219951286, 61.46049967264873715, 39.21067981925356349 ) ) ;
#2895 = AXIS2_PLACEMENT_3D ( 'NONE', #5494, #19276, #2515 ) ;
#2896 = EDGE_LOOP ( 'NONE', ( #11907, #1390, #19035, #5979 ) ) ;
#2897 = CARTESIAN_POINT ( 'NONE',  ( 45.74753988029933538, 79.42977050742732104, 37.97664729208901946 ) ) ;
#2898 = CARTESIAN_POINT ( 'NONE',  ( -143.8425227516148084, -192.9584106276440423, 55.19815736654470584 ) ) ;
#2899 = CARTESIAN_POINT ( 'NONE',  ( 10.16827731527805767, 110.2528774685086574, 8.767718578943870966 ) ) ;
#2900 = CARTESIAN_POINT ( 'NONE',  ( -143.8425227516148084, -186.3584106276440480, 44.11586579668791330 ) ) ;
#2901 = VECTOR ( 'NONE', #20014, 1000.000000000000000 ) ;
#2902 = ORIENTED_EDGE ( 'NONE', *, *, #10237, .T. ) ;
#2903 = ADVANCED_FACE ( 'NONE', ( #8379 ), #20176, .T. ) ;
#2904 = LINE ( 'NONE', #16229, #19073 ) ;
#2905 = CARTESIAN_POINT ( 'NONE',  ( 39.42975644700377558, 126.6797705074273210, 36.81289934271958941 ) ) ;
#2906 = ORIENTED_EDGE ( 'NONE', *, *, #7281, .F. ) ;
#2907 = ADVANCED_FACE ( 'NONE', ( #16405 ), #1428, .F. ) ;
#2908 =( NAMED_UNIT ( * ) PLANE_ANGLE_UNIT ( ) SI_UNIT ( $, .RADIAN. ) );
#2909 = ORIENTED_EDGE ( 'NONE', *, *, #7540, .T. ) ;
#2910 = CARTESIAN_POINT ( 'NONE',  ( 47.43856463449118621, 124.8797705074273239, 34.21067981925357060 ) ) ;
#2911 = CARTESIAN_POINT ( 'NONE',  ( 43.01140435219953417, 138.5344580088726048, 39.21067981925356349 ) ) ;
#2912 = CARTESIAN_POINT ( 'NONE',  ( 43.01140435219951286, 88.12977050742732388, 38.86567161673127657 ) ) ;
#2913 = CARTESIAN_POINT ( 'NONE',  ( 44.55648932407425633, 64.88445800887257064, 29.45539723777780239 ) ) ;
#2914 = DIRECTION ( 'NONE',  ( 0.9393725726208708160, 0.3428981916074316794, -0.000000000000000000 ) ) ;
#2915 = CYLINDRICAL_SURFACE ( 'NONE', #19100, 4.999999999999997335 ) ;
#2916 = CARTESIAN_POINT ( 'NONE',  ( -157.6495955161842062, -191.0391397928654271, 58.16351966513671812 ) ) ;
#2917 = CARTESIAN_POINT ( 'NONE',  ( 41.46631938032478359, 156.1104996726487570, 29.45539723777780239 ) ) ;
#2918 = LINE ( 'NONE', #6560, #10778 ) ;
#2919 = CARTESIAN_POINT ( 'NONE',  ( -157.2955611005346270, -191.3438272943106995, 41.63779006702063867 ) ) ;
#2920 = APPLICATION_PROTOCOL_DEFINITION ( 'draft international standard', 'automotive_design', 1998, #4077 ) ;
#2921 = CARTESIAN_POINT ( 'NONE',  ( 41.46631938032478359, 120.3844580088725849, 38.96596240072933170 ) ) ;
#2922 = CARTESIAN_POINT ( 'NONE',  ( 46.59305225739526435, 106.5797705074273125, 36.81289934271958941 ) ) ;
#2923 = CARTESIAN_POINT ( 'NONE',  ( 29.27949416537561333, 144.5119445999418986, 23.32977622066093204 ) ) ;
#2924 = CARTESIAN_POINT ( 'NONE',  ( -159.0959885057557983, -185.1938272943107222, 44.11586579668791330 ) ) ;
#2925 = CARTESIAN_POINT ( 'NONE',  ( 46.59305225739526435, 91.31518717409399244, 36.81289934271958941 ) ) ;
#2926 = CARTESIAN_POINT ( 'NONE',  ( 156.1725454929228079, -61.68114226949890622, -16.21320343559643717 ) ) ;
#2927 = VERTEX_POINT ( 'NONE', #11262 ) ;
#2928 = CYLINDRICAL_SURFACE ( 'NONE', #11527, 4.999999999999997335 ) ;
#2929 = CARTESIAN_POINT ( 'NONE',  ( 72.98789752971651978, 103.3738663174133023, 6.148623012889737005 ) ) ;
#2930 = CARTESIAN_POINT ( 'NONE',  ( 69.30627838890079317, 109.9422389716749535, -13.93421298911417416 ) ) ;
#2931 = CARTESIAN_POINT ( 'NONE',  ( 38.58424406990785371, 69.22977050742731819, 32.77220824515697473 ) ) ;
#2932 = EDGE_LOOP ( 'NONE', ( #3098, #5240 ) ) ;
#2933 = EDGE_LOOP ( 'NONE', ( #12689, #2522, #10282, #17668 ) ) ;
#2934 = CARTESIAN_POINT ( 'NONE',  ( 45.74753988029933538, 154.4297705074272926, 37.97664729208901946 ) ) ;
#2935 = LINE ( 'NONE', #21135, #17207 ) ;
#2936 = CARTESIAN_POINT ( 'NONE',  ( 46.10157429594899270, 113.6604996726487542, 29.95742577749337343 ) ) ;
#2937 = CARTESIAN_POINT ( 'NONE',  ( 38.58424406990784661, 66.26518717409400949, 35.64915139335016647 ) ) ;
#2938 = CARTESIAN_POINT ( 'NONE',  ( -156.1828684652451500, -155.6591478762520921, 41.49287016839741682 ) ) ;
#2939 = CARTESIAN_POINT ( 'NONE',  ( -143.8425227516148084, -162.6938272943107222, 55.19815736654470584 ) ) ;
#2940 = CARTESIAN_POINT ( 'NONE',  ( -161.4692556286853176, -175.5630981290893260, 49.65701158161630957 ) ) ;
#2941 = CARTESIAN_POINT ( 'NONE',  ( 48.01140435219951996, 151.2844580088725763, 34.21067981925357060 ) ) ;
#2942 = CARTESIAN_POINT ( 'NONE',  ( 41.64333658814960870, 132.9797705074273324, 38.42115945441014446 ) ) ;
#2943 = CARTESIAN_POINT ( 'NONE',  ( 13.97286934428321103, 138.1879231288898495, 15.71574578848041881 ) ) ;
#2944 = CARTESIAN_POINT ( 'NONE',  ( 46.59305225739526435, 130.3151871740940067, 36.81289934271958941 ) ) ;
#2945 = EDGE_CURVE ( 'NONE', #7555, #1878, #9921, .T. ) ;
#2946 = DIRECTION ( 'NONE',  ( 1.000000000000000000, 0.000000000000000000, 0.000000000000000000 ) ) ;
#2947 = FACE_OUTER_BOUND ( 'NONE', #18981, .T. ) ;
#2948 = CARTESIAN_POINT ( 'NONE',  ( 46.10157429594899270, 139.7604996726487627, 38.46393386101375711 ) ) ;
#2949 = DIRECTION ( 'NONE',  ( -1.000000000000000000, 0.000000000000000000, 0.000000000000000000 ) ) ;
#2950 = CARTESIAN_POINT ( 'NONE',  ( 15.78326802858598299, 112.2624592280589439, 21.86641499745291028 ) ) ;
#2951 = CARTESIAN_POINT ( 'NONE',  ( -143.3790856849358306, -186.6891397928654612, 43.77915905869157598 ) ) ;
#2952 = VECTOR ( 'NONE', #1787, 1000.000000000000114 ) ;
#2953 = ORIENTED_EDGE ( 'NONE', *, *, #7751, .T. ) ;
#2954 = LINE ( 'NONE', #10911, #8544 ) ;
#2955 = VERTEX_POINT ( 'NONE', #3419 ) ;
#2956 = CARTESIAN_POINT ( 'NONE',  ( 43.01140435219951286, 86.03445800887257633, 28.95336869806222779 ) ) ;
#2957 = DIRECTION ( 'NONE',  ( 0.000000000000000000, -1.000000000000000000, 0.000000000000000000 ) ) ;
#2958 = ADVANCED_FACE ( 'NONE', ( #16298 ), #19724, .T. ) ;
#2959 = CARTESIAN_POINT ( 'NONE',  ( 41.46631938032478359, 144.1104996726487570, 29.45539723777780239 ) ) ;
#2961 = CARTESIAN_POINT ( 'NONE',  ( 42.16380956469475194, 91.80013758078052888, 8.446644326836734606 ) ) ;
#2960 = CARTESIAN_POINT ( 'NONE',  ( 41.64333658814960870, 93.71518717409401233, 38.42115945441014446 ) ) ;
#2962 = CARTESIAN_POINT ( 'NONE',  ( -148.5561028927606344, -172.2584106276440536, 58.62277379824867296 ) ) ;
#2963 = CARTESIAN_POINT ( 'NONE',  ( -143.8425227516148084, -189.6938272943107222, 55.19815736654470584 ) ) ;
#2965 = CARTESIAN_POINT ( 'NONE',  ( 43.01140435219957681, 71.03445800887256212, 29.21067981925356705 ) ) ;
#2964 = DIRECTION ( 'NONE',  ( -1.000000000000000000, 0.000000000000000000, 0.000000000000000000 ) ) ;
#2966 = CARTESIAN_POINT ( 'NONE',  ( 38.01140435219952707, 105.8604996726487428, 35.83527830041809636 ) ) ;
#2967 = ADVANCED_BREP_SHAPE_REPRESENTATION ( '', ( #7648, #12657 ), #7388 ) ;
#2968 = CARTESIAN_POINT ( 'NONE',  ( -143.3790856849358306, -174.6891397928654612, 43.77915905869157598 ) ) ;
#2969 = CARTESIAN_POINT ( 'NONE',  ( 44.55648932407425633, 80.81049967264873146, 29.45539723777780239 ) ) ;
#2970 = CARTESIAN_POINT ( 'NONE',  ( 44.37947211624943833, 65.21518717409399812, 30.00020018409699318 ) ) ;
#2971 = CARTESIAN_POINT ( 'NONE',  ( 75.80354157443048280, 110.0810758630161672, 5.910575721798123183 ) ) ;
#2972 = AXIS2_PLACEMENT_3D ( 'NONE', #5225, #5530, #11012 ) ;
#2973 = CARTESIAN_POINT ( 'NONE',  ( 44.37947211624943833, 151.0151871740940237, 38.42115945441014446 ) ) ;
#2974 = CARTESIAN_POINT ( 'NONE',  ( -159.0959885057557983, -160.5938272943107279, 55.19815736654470584 ) ) ;
#2975 = CARTESIAN_POINT ( 'NONE',  ( -148.5561028927606344, -186.0584106276440650, 40.69124936498395328 ) ) ;
#2976 = ORIENTED_EDGE ( 'NONE', *, *, #9209, .F. ) ;
#2977 = CARTESIAN_POINT ( 'NONE',  ( 47.43856463449117911, 73.76518717409398107, 32.77220824515697473 ) ) ;
#2978 = CARTESIAN_POINT ( 'NONE',  ( -159.0959885057557983, -169.8584106276440764, 55.19815736654470584 ) ) ;
#2979 = CARTESIAN_POINT ( 'NONE',  ( 8.737656864016759783, 121.5850998216562431, 22.14420391595633220 ) ) ;
#2980 = LINE ( 'NONE', #6398, #9178 ) ;
#2981 = CARTESIAN_POINT ( 'NONE',  ( 38.58424406990784661, 137.9651871740939839, 32.77220824515698183 ) ) ;
#2982 = EDGE_CURVE ( 'NONE', #9530, #10777, #9705, .T. ) ;
#2983 = CARTESIAN_POINT ( 'NONE',  ( 69.52170837389681424, 98.37355370181180092, -13.65637406972050272 ) ) ;
#2984 = ORIENTED_EDGE ( 'NONE', *, *, #11356, .F. ) ;
#2985 = VERTEX_POINT ( 'NONE', #16627 ) ;
#2986 = CARTESIAN_POINT ( 'NONE',  ( 69.85845278386915425, 111.2786852186620621, 13.01367670771671747 ) ) ;
#2987 = ORIENTED_EDGE ( 'NONE', *, *, #15449, .T. ) ;
#2988 = LINE ( 'NONE', #21521, #3748 ) ;
#2989 = CARTESIAN_POINT ( 'NONE',  ( 40.27526882409969033, 69.82977050742729830, 37.97664729208901946 ) ) ;
#2991 = CARTESIAN_POINT ( 'NONE',  ( 31.84750084766683287, 94.01163676417708359, 0.8705387173494113506 ) ) ;
#2990 = CARTESIAN_POINT ( 'NONE',  ( 41.64333658814960870, 129.7151871740940123, 38.42115945441014446 ) ) ;
#2992 = CARTESIAN_POINT ( 'NONE',  ( 47.05648932407426344, 92.51049967264873430, 31.27175355779120025 ) ) ;
#2993 = CARTESIAN_POINT ( 'NONE',  ( -151.4692556286852891, -196.9891397928655010, 49.65701158161630957 ) ) ;
#2994 = VECTOR ( 'NONE', #5145, 1000.000000000000000 ) ;
#2995 = ADVANCED_FACE ( 'NONE', ( #14969 ), #21608, .F. ) ;
#2996 = CARTESIAN_POINT ( 'NONE',  ( 39.24730198293589467, 95.19097405389743471, 30.90345582088290044 ) ) ;
#2997 = CARTESIAN_POINT ( 'NONE',  ( 38.96631938032478359, 139.0104996726487627, 37.14960608071593384 ) ) ;
#2998 = ADVANCED_FACE ( 'NONE', ( #1536 ), #13334, .F. ) ;
#2999 = CARTESIAN_POINT ( 'NONE',  ( 43.01140435219951286, 84.86518717409398960, 38.86567161673127657 ) ) ;
#3000 = CARTESIAN_POINT ( 'NONE',  ( 43.01140435219957681, 68.96049967264870872, 29.21067981925356705 ) ) ;
#3001 = CARTESIAN_POINT ( 'NONE',  ( 43.80332655382221674, 108.6113394311928460, 39.21067981925355639 ) ) ;
#3002 = CARTESIAN_POINT ( 'NONE',  ( 43.80332655382220253, 62.88361825032846752, 29.21067981925356705 ) ) ;
#3003 = ORIENTED_EDGE ( 'NONE', *, *, #988, .F. ) ;
#3004 = CARTESIAN_POINT ( 'NONE',  ( 44.37947211624943833, 79.27977050742731535, 38.42115945441014446 ) ) ;
#3005 = CARTESIAN_POINT ( 'NONE',  ( -159.0959885057557983, -191.4584106276440423, 44.11586579668791330 ) ) ;
#3006 = EDGE_CURVE ( 'NONE', #10856, #8233, #16511, .T. ) ;
#3007 = CARTESIAN_POINT ( 'NONE',  ( 48.17517050666977241, 153.7480039124125994, 4.005852979123367241 ) ) ;
#3008 = CARTESIAN_POINT ( 'NONE',  ( -142.0420953463935803, -183.8084106276440366, 52.72008163687743831 ) ) ;
#3009 = ORIENTED_EDGE ( 'NONE', *, *, #8423, .F. ) ;
#3010 = FACE_OUTER_BOUND ( 'NONE', #8960, .T. ) ;
#3011 = PLANE ( 'NONE',  #9235 ) ;
#3012 = CARTESIAN_POINT ( 'NONE',  ( 39.42975644700377558, 120.0797705074273267, 31.60846029578754468 ) ) ;
#3013 = ORIENTED_EDGE ( 'NONE', *, *, #14327, .F. ) ;
#3014 = AXIS2_PLACEMENT_3D ( 'NONE', #17733, #19730, #2639 ) ;
#3015 = EDGE_LOOP ( 'NONE', ( #12043, #12503, #17690, #7873 ) ) ;
#3016 = CARTESIAN_POINT ( 'NONE',  ( 41.64333658814960870, 119.7797705074273296, 30.00020018409699318 ) ) ;
#3017 = CARTESIAN_POINT ( 'NONE',  ( 43.01140435219951286, 59.03445800887258343, 29.21067981925356705 ) ) ;
#3018 = CARTESIAN_POINT ( 'NONE',  ( 39.42975644700377558, 90.67977050742732104, 36.81289934271958941 ) ) ;
#3019 = CARTESIAN_POINT ( 'NONE',  ( 38.58424406990786082, 156.1151871740940180, 34.21067981925357060 ) ) ;
#3020 =( BOUNDED_CURVE ( )  B_SPLINE_CURVE ( 2, ( #8761, #6891, #15036, #1595, #1817, #3581, #11840, #6791, #10413, #18887, #3362, #379, #16796 ),
 .UNSPECIFIED., .F., .F. ) 
 B_SPLINE_CURVE_WITH_KNOTS ( ( 3, 2, 2, 2, 2, 2, 3 ),
 ( 0.01785714285714286656, 0.02142857142857142877, 0.02857142857142857054, 0.03571428571428571230, 0.04285714285714285754, 0.05000000000000000278, 0.05357142857142854764 ),
 .UNSPECIFIED. ) 
 CURVE ( )  GEOMETRIC_REPRESENTATION_ITEM ( )  RATIONAL_B_SPLINE_CURVE ( ( 0.9755282581475768211, 0.9755282581475768211, 1.000000000000000000, 0.9510565162951535312, 1.000000000000000000, 0.9510565162951535312, 1.000000000000000000, 0.9510565162951535312, 1.000000000000000000, 0.9510565162951535312, 1.000000000000000000, 0.9755282581475768211, 0.9755282581475765991 ) ) 
 REPRESENTATION_ITEM ( '' )  );
#3021 = VECTOR ( 'NONE', #4706, 1000.000000000000000 ) ;
#3022 = CARTESIAN_POINT ( 'NONE',  ( -176.9699209214867892, -37.13255853780189852, 30.00000000000000000 ) ) ;
#3023 = DIRECTION ( 'NONE',  ( 0.9387810623359078566, 0.3426822732243069436, 0.03548206049944095664 ) ) ;
#3024 = LINE ( 'NONE', #18003, #3512 ) ;
#3025 = CARTESIAN_POINT ( 'NONE',  ( -143.3790856849358306, -192.6891397928654897, 43.77915905869157598 ) ) ;
#3026 = DIRECTION ( 'NONE',  ( -0.4938165983075539223, 0.8695660798558991766, 0.000000000000000000 ) ) ;
#3027 = CARTESIAN_POINT ( 'NONE',  ( 39.92123440845005433, 103.1604996726487258, 38.46393386101375711 ) ) ;
#3028 = CARTESIAN_POINT ( 'NONE',  ( -151.4692556286852891, -194.6438272943107393, 39.74470866294723947 ) ) ;
#3029 = CARTESIAN_POINT ( 'NONE',  ( 46.10157429594899270, 118.7344580088725650, 29.95742577749337343 ) ) ;
#3030 = CARTESIAN_POINT ( 'NONE',  ( 45.74753988029933538, 103.4297705074273210, 37.97664729208901946 ) ) ;
#3031 = CARTESIAN_POINT ( 'NONE',  ( 32.03768905382736421, 145.5187656067679711, 23.43402463578956585 ) ) ;
#3032 = CARTESIAN_POINT ( 'NONE',  ( -151.4692556286852891, -182.6438272943107108, 39.74470866294723947 ) ) ;
#3033 = CARTESIAN_POINT ( 'NONE',  ( 47.43856463449117911, 85.76518717409398107, 32.77220824515697473 ) ) ;
#3034 = CARTESIAN_POINT ( 'NONE',  ( 43.01140435219954838, 133.4604996726487514, 39.21067981925356349 ) ) ;
#3035 = ORIENTED_EDGE ( 'NONE', *, *, #11167, .T. ) ;
#3036 = CARTESIAN_POINT ( 'NONE',  ( 43.01140435219953417, 138.5344580088726048, 39.21067981925356349 ) ) ;
#3037 = CARTESIAN_POINT ( 'NONE',  ( 15.97061701817242785, 140.8453463817331794, 16.82122940411608170 ) ) ;
#3038 = CARTESIAN_POINT ( 'NONE',  ( 14.89151287784495281, 119.8505320279099209, -10.83935810001172229 ) ) ;
#3039 = CARTESIAN_POINT ( 'NONE',  ( 38.58424406990785371, 63.22977050742731109, 32.77220824515697473 ) ) ;
#3040 = EDGE_LOOP ( 'NONE', ( #14449, #15905, #15988, #16475 ) ) ;
#3041 = EDGE_LOOP ( 'NONE', ( #18081, #20830, #4851, #15021 ) ) ;
#3042 = CARTESIAN_POINT ( 'NONE',  ( 43.01140435219951286, 148.1297705074272812, 38.86567161673127657 ) ) ;
#3043 = AXIS2_PLACEMENT_3D ( 'NONE', #14344, #7530, #10618 ) ;
#3044 = DIRECTION ( 'NONE',  ( -1.915514545828640705E-16, -7.041092946335507105E-17, -1.000000000000000000 ) ) ;
#3045 = ADVANCED_FACE ( 'NONE', ( #4840 ), #4957, .T. ) ;
#3046 = EDGE_CURVE ( 'NONE', #17658, #9281, #3864, .T. ) ;
#3047 = CARTESIAN_POINT ( 'NONE',  ( 43.01140435219951286, 112.4604996726487514, 39.46799094044489209 ) ) ;
#3048 = CARTESIAN_POINT ( 'NONE',  ( 44.37947211624943833, 73.01518717409399528, 38.42115945441014446 ) ) ;
#3049 = DIRECTION ( 'NONE',  ( 1.000000000000000000, 0.000000000000000000, -0.000000000000000000 ) ) ;
#3050 = CARTESIAN_POINT ( 'NONE',  ( -142.0420953463935803, -159.2438272943107336, 46.59394152635518083 ) ) ;
#3051 = CARTESIAN_POINT ( 'NONE',  ( 134.6380592378700101, 268.5785371414991687, -3.999999999999996447 ) ) ;
#3052 = CARTESIAN_POINT ( 'NONE',  ( -141.4692556286852891, -173.9130981290893203, 46.40781461928724383 ) ) ;
#3053 = CARTESIAN_POINT ( 'NONE',  ( 39.92123440845005433, 111.2604996726487343, 29.95742577749336988 ) ) ;
#3054 = CARTESIAN_POINT ( 'NONE',  ( 39.42975644700377558, 135.0797705074272983, 31.60846029578754468 ) ) ;
#3055 = CARTESIAN_POINT ( 'NONE',  ( 52.27439898384277939, 152.9467924839493946, 17.14431721725165758 ) ) ;
#3056 = CONICAL_SURFACE ( 'NONE', #5867, 9.000000000000007105, 0.7853981633974346233 ) ;
#3057 = CARTESIAN_POINT ( 'NONE',  ( 47.43856463449117911, 115.4651871740940123, 35.64915139335015937 ) ) ;
#3058 = CARTESIAN_POINT ( 'NONE',  ( -151.4692556286852891, -196.9891397928655010, 39.65701158161630246 ) ) ;
#3059 = FACE_OUTER_BOUND ( 'NONE', #1936, .T. ) ;
#3060 = CARTESIAN_POINT ( 'NONE',  ( 147.5268905834513475, 193.0332408774651185, 14.00000000000001776 ) ) ;
#3061 = CARTESIAN_POINT ( 'NONE',  ( 38.96631938032478359, 135.4104996726487400, 31.27175355779120025 ) ) ;
#3062 = CARTESIAN_POINT ( 'NONE',  ( 31.34884810169724645, 145.5825485123889109, -10.55804779818428862 ) ) ;
#3063 = CARTESIAN_POINT ( 'NONE',  ( 141.4773229304660447, 84.89323405393692212, 4.000000000000021316 ) ) ;
#3064 = CARTESIAN_POINT ( 'NONE',  ( 38.58424406990785371, 96.22977050742730398, 32.77220824515697473 ) ) ;
#3065 = VERTEX_POINT ( 'NONE', #20599 ) ;
#3066 = DIRECTION ( 'NONE',  ( 0.000000000000000000, 0.000000000000000000, 1.000000000000000000 ) ) ;
#3067 = VERTEX_POINT ( 'NONE', #6836 ) ;
#3068 = CARTESIAN_POINT ( 'NONE',  ( 47.05648932407426344, 79.58445800887257349, 31.27175355779120025 ) ) ;
#3069 = CARTESIAN_POINT ( 'NONE',  ( 157.5268905834513475, 193.0332408774651185, 4.000000000000021316 ) ) ;
#3070 = ADVANCED_FACE ( 'NONE', ( #426 ), #15312, .T. ) ;
#3071 = CARTESIAN_POINT ( 'NONE',  ( 38.01140435219952707, 135.7104996726487514, 34.21067981925357060 ) ) ;
#3073 = CARTESIAN_POINT ( 'NONE',  ( 65.57965399412842089, 103.1314161556117028, 7.375186511277089352 ) ) ;
#3072 = CARTESIAN_POINT ( 'NONE',  ( 47.43856463449117200, 100.7651871740939953, 32.77220824515698183 ) ) ;
#3074 = CARTESIAN_POINT ( 'NONE',  ( -81.61981105773979550, 604.5992151483073940, -23.16745088979876499 ) ) ;
#3075 = CARTESIAN_POINT ( 'NONE',  ( -151.4692556286852891, -164.9084106276440593, 39.74470866294723947 ) ) ;
#3076 = CARTESIAN_POINT ( 'NONE',  ( -160.8964159109769696, -193.8938272943107393, 49.65701158161630957 ) ) ;
#3078 = CARTESIAN_POINT ( 'NONE',  ( 111.4021762516569964, 137.5714195593754710, 272.0939500981630204 ) ) ;
#3077 = CARTESIAN_POINT ( 'NONE',  ( -161.4692556286852891, -178.4130981290893203, 52.90620854394536821 ) ) ;
#3079 = DIRECTION ( 'NONE',  ( 5.966140889015784385E-16, 0.000000000000000000, -1.000000000000000000 ) ) ;
#3080 = CARTESIAN_POINT ( 'NONE',  ( -148.3790856849358306, -175.5891397928654669, 59.16757674456786020 ) ) ;
#3081 = CARTESIAN_POINT ( 'NONE',  ( 11.17254549292281318, -61.68114226949890622, 20.00000000000000355 ) ) ;
#3082 =( BOUNDED_CURVE ( )  B_SPLINE_CURVE ( 2, ( #19330, #17770, #11165, #16008, #7665, #1140, #14574, #1033, #5877, #21317, #14466, #6203, #2676 ),
 .UNSPECIFIED., .F., .F. ) 
 B_SPLINE_CURVE_WITH_KNOTS ( ( 3, 2, 2, 2, 2, 2, 3 ),
 ( 0.3308823529411764608, 0.3323529411764705732, 0.3352941176470587981, 0.3382352941176470784, 0.3411764705882353033, 0.3441176470588235281, 0.3455882352941176405 ),
 .UNSPECIFIED. ) 
 CURVE ( )  GEOMETRIC_REPRESENTATION_ITEM ( )  RATIONAL_B_SPLINE_CURVE ( ( 0.9755282581475768211, 0.9755282581475768211, 1.000000000000000000, 0.9510565162951535312, 1.000000000000000000, 0.9510565162951535312, 1.000000000000000000, 0.9510565162951535312, 1.000000000000000000, 0.9510565162951535312, 1.000000000000000000, 0.9755282581475768211, 0.9755282581475768211 ) ) 
 REPRESENTATION_ITEM ( '' )  );
#3083 = CARTESIAN_POINT ( 'NONE',  ( 44.37947211624943833, 61.01518717409400239, 38.42115945441014446 ) ) ;
#3084 = CARTESIAN_POINT ( 'NONE',  ( 83.67254549292280785, -61.68114226949890622, 20.00000000000000355 ) ) ;
#3085 = CARTESIAN_POINT ( 'NONE',  ( 66.76198117565915879, 95.25264312590786631, -0.5179092472497510702 ) ) ;
#3086 = CARTESIAN_POINT ( 'NONE',  ( 44.37947211624943833, 145.0151871740939953, 38.42115945441014446 ) ) ;
#3087 = AXIS2_PLACEMENT_3D ( 'NONE', #5335, #10087, #8763 ) ;
#3088 = CARTESIAN_POINT ( 'NONE',  ( -145.6429501568359797, -165.8438272943107563, 57.67623309621198047 ) ) ;
#3089 = CARTESIAN_POINT ( 'NONE',  ( -154.3824083646099439, -182.7584106276440536, 40.69124936498395328 ) ) ;
#3090 = ORIENTED_EDGE ( 'NONE', *, *, #18510, .F. ) ;
#3091 = CARTESIAN_POINT ( 'NONE',  ( 38.58424406990785371, 72.26518717409398107, 35.64915139335015937 ) ) ;
#3092 = CARTESIAN_POINT ( 'NONE',  ( -160.8964159109769696, -170.3084106276440082, 46.59394152635518793 ) ) ;
#3093 = CARTESIAN_POINT ( 'NONE',  ( 42.43310160994198554, 85.59785666124599857, 20.35848333119881914 ) ) ;
#3094 = AXIS2_PLACEMENT_3D ( 'NONE', #3137, #9543, #6559 ) ;
#3095 = SURFACE_STYLE_FILL_AREA ( #10929 ) ;
#3096 = CARTESIAN_POINT ( 'NONE',  ( 47.43856463449117200, 124.4651871740939839, 35.64915139335016647 ) ) ;
#3097 = CARTESIAN_POINT ( 'NONE',  ( 27.13677837140323490, 150.1474281128565167, -2.704124018797368301 ) ) ;
#3098 = ORIENTED_EDGE ( 'NONE', *, *, #12468, .F. ) ;
#3099 = ORIENTED_EDGE ( 'NONE', *, *, #7039, .F. ) ;
#3100 = CARTESIAN_POINT ( 'NONE',  ( 65.77248029998415291, 103.2585056976580091, 13.37079068582577435 ) ) ;
#3101 = ORIENTED_EDGE ( 'NONE', *, *, #3982, .T. ) ;
#3102 = CARTESIAN_POINT ( 'NONE',  ( 39.92123440845004723, 108.2344580088725792, 38.46393386101376421 ) ) ;
#3103 = FACE_OUTER_BOUND ( 'NONE', #3430, .T. ) ;
#3104 = CARTESIAN_POINT ( 'NONE',  ( 43.01140435219951286, 62.62977050742732388, 29.55568802177586463 ) ) ;
#3106 = CARTESIAN_POINT ( 'NONE',  ( 51.84853669763433004, 93.12814091139611605, 7.061107544354192633 ) ) ;
#3105 = CARTESIAN_POINT ( 'NONE',  ( 45.74753988029933538, 122.0651871740940209, 30.44471234641811819 ) ) ;
#3107 = CARTESIAN_POINT ( 'NONE',  ( 39.92123440845004723, 85.16049967264873999, 38.46393386101376421 ) ) ;
#3108 = CARTESIAN_POINT ( 'NONE',  ( 14.48810111090402941, 100.9784058478479523, 15.43442115621699529 ) ) ;
#3109 = CYLINDRICAL_SURFACE ( 'NONE', #17734, 4.999999999999997335 ) ;
#3110 = DIRECTION ( 'NONE',  ( 0.000000000000000000, -1.000000000000000000, 0.000000000000000000 ) ) ;
#3111 = CARTESIAN_POINT ( 'NONE',  ( 47.43856463449117200, 85.46518717409399812, 35.64915139335016647 ) ) ;
#3112 = UNCERTAINTY_MEASURE_WITH_UNIT (LENGTH_MEASURE( 1.000000000000000082E-05 ), #15176, 'distance_accuracy_value', 'NONE');
#3113 = CARTESIAN_POINT ( 'NONE',  ( 141.1725454929228079, -61.68114226949890622, 30.00000000000000000 ) ) ;
#3114 = CARTESIAN_POINT ( 'NONE',  ( -159.5594255724347761, -185.1891397928654612, 55.53486410454104316 ) ) ;
#3115 = EDGE_LOOP ( 'NONE', ( #387, #5902 ) ) ;
#3116 = CARTESIAN_POINT ( 'NONE',  ( 39.42975644700377558, 69.07977050742732672, 31.60846029578754468 ) ) ;
#3117 = CARTESIAN_POINT ( 'NONE',  ( -159.0959885057557983, -157.5938272943107279, 55.19815736654470584 ) ) ;
#3118 = CARTESIAN_POINT ( 'NONE',  ( 71.03835150376274044, 100.2492380157770526, 6.267546321443639989 ) ) ;
#3119 = CARTESIAN_POINT ( 'NONE',  ( -148.5561028927606344, -186.0584106276440650, 40.69124936498395328 ) ) ;
#3120 = EDGE_LOOP ( 'NONE', ( #3971, #3699, #6691, #12257 ) ) ;
#3121 = CARTESIAN_POINT ( 'NONE',  ( -154.5594255724347761, -160.8891397928654499, 59.16757674456785310 ) ) ;
#3122 = ADVANCED_FACE ( 'NONE', ( #204 ), #18619, .T. ) ;
#3123 = CARTESIAN_POINT ( 'NONE',  ( 43.01140435219951286, 122.9604996726487371, 29.21067981925356705 ) ) ;
#3124 = CARTESIAN_POINT ( 'NONE',  ( 40.27526882409969744, 113.9297705074273068, 30.44471234641812174 ) ) ;
#3125 = CARTESIAN_POINT ( 'NONE',  ( 75.10802748102119608, 108.0013139708956800, -8.018167963582932600 ) ) ;
#3126 = EDGE_LOOP ( 'NONE', ( #4259, #8088, #5351, #15639 ) ) ;
#3127 = CARTESIAN_POINT ( 'NONE',  ( 48.01140435219951996, 88.28445800887257633, 34.21067981925357060 ) ) ;
#3128 = ORIENTED_EDGE ( 'NONE', *, *, #7265, .F. ) ;
#3129 = CARTESIAN_POINT ( 'NONE',  ( 41.64333658814960870, 116.7797705074273296, 30.00020018409699318 ) ) ;
#3130 = CARTESIAN_POINT ( 'NONE',  ( 43.01140435219951996, 170.7104996726487514, 34.21067981925357060 ) ) ;
#3131 = CARTESIAN_POINT ( 'NONE',  ( 47.43856463449117200, 85.72977050742731819, 35.64915139335016647 ) ) ;
#3132 = CARTESIAN_POINT ( 'NONE',  ( 38.58424406990784661, 149.9651871740939555, 32.77220824515698183 ) ) ;
#3133 = CARTESIAN_POINT ( 'NONE',  ( 156.5548063637509415, 177.1359029563629406, -29.99999999999997868 ) ) ;
#3134 = CARTESIAN_POINT ( 'NONE',  ( -151.4692556286852607, -183.8130981290892692, 59.65701158161632378 ) ) ;
#3135 = DIRECTION ( 'NONE',  ( -0.9385982292947087080, -0.3450121214752278620, 0.000000000000000000 ) ) ;
#3136 = CARTESIAN_POINT ( 'NONE',  ( -151.4692556286852891, -178.7391397928655010, 60.17163382399899518 ) ) ;
#3137 = CARTESIAN_POINT ( 'NONE',  ( -151.4692556286852891, -195.9891397928654726, 49.65701158161630957 ) ) ;
#3138 = CARTESIAN_POINT ( 'NONE',  ( 48.01140435219951996, 94.28445800887259054, 34.21067981925357060 ) ) ;
#3139 = CARTESIAN_POINT ( 'NONE',  ( -151.4692556286852891, -190.1438272943107393, 59.56931450028537967 ) ) ;
#3140 = VECTOR ( 'NONE', #5913, 1000.000000000000000 ) ;
#3141 = CARTESIAN_POINT ( 'NONE',  ( 38.01140435219951996, 122.9344580088725962, 35.83527830041810347 ) ) ;
#3142 = CARTESIAN_POINT ( 'NONE',  ( 38.58424406990784661, 93.52977050742731535, 35.64915139335016647 ) ) ;
#3143 = CARTESIAN_POINT ( 'NONE',  ( 51.52566954327383542, 92.93877768781105431, 20.08059929855049219 ) ) ;
#3144 = CARTESIAN_POINT ( 'NONE',  ( -160.8964159109769696, -184.8938272943107393, 49.65701158161630957 ) ) ;
#3145 = CARTESIAN_POINT ( 'NONE',  ( 43.01140435219951286, 90.86518717409400381, 38.86567161673127657 ) ) ;
#3146 = CARTESIAN_POINT ( 'NONE',  ( 41.46631938032478359, 84.11049967264874283, 29.45539723777780239 ) ) ;
#3147 = VERTEX_POINT ( 'NONE', #19051 ) ;
#3148 = CARTESIAN_POINT ( 'NONE',  ( 43.01140435219951286, 127.4604996726487229, 39.21067981925356349 ) ) ;
#3149 = CARTESIAN_POINT ( 'NONE',  ( 52.46025766099742071, 152.8098426157893925, 11.14871012209260748 ) ) ;
#3150 = CARTESIAN_POINT ( 'NONE',  ( 70.62278752756289180, 114.5844828164671441, -0.1247842873985126749 ) ) ;
#3151 = CARTESIAN_POINT ( 'NONE',  ( 47.43856463449117200, 103.4651871740939839, 35.64915139335016647 ) ) ;
#3152 = CARTESIAN_POINT ( 'NONE',  ( 44.37947211624943833, 70.27977050742731535, 38.42115945441014446 ) ) ;
#3153 =( BOUNDED_CURVE ( )  B_SPLINE_CURVE ( 2, ( #8472, #3506, #10447, #20580, #5466, #5572, #5366, #7250, #13525, #11870, #10552, #18708, #3615 ),
 .UNSPECIFIED., .F., .F. ) 
 B_SPLINE_CURVE_WITH_KNOTS ( ( 3, 2, 2, 2, 2, 2, 3 ),
 ( 0.2678571428571429047, 0.2714285714285714080, 0.2785714285714285809, 0.2857142857142856984, 0.2928571428571428714, 0.2999999999999999889, 0.3035714285714286031 ),
 .UNSPECIFIED. ) 
 CURVE ( )  GEOMETRIC_REPRESENTATION_ITEM ( )  RATIONAL_B_SPLINE_CURVE ( ( 0.9755282581475768211, 0.9755282581475771542, 1.000000000000000000, 0.9510565162951535312, 1.000000000000000000, 0.9510565162951535312, 1.000000000000000000, 0.9510565162951535312, 1.000000000000000000, 0.9510565162951535312, 1.000000000000000000, 0.9755282581475765991, 0.9755282581475768211 ) ) 
 REPRESENTATION_ITEM ( '' )  );
#3154 = ORIENTED_EDGE ( 'NONE', *, *, #5582, .F. ) ;
#3155 = CARTESIAN_POINT ( 'NONE',  ( 46.59305225739526435, 149.1797705074273210, 31.60846029578754468 ) ) ;
#3156 = EDGE_CURVE ( 'NONE', #7690, #15802, #9916, .T. ) ;
#3157 = CARTESIAN_POINT ( 'NONE',  ( 39.42975644700377558, 96.67977050742732104, 36.81289934271958941 ) ) ;
#3159 = EDGE_CURVE ( 'NONE', #2574, #14607, #20383, .T. ) ;
#3158 = CARTESIAN_POINT ( 'NONE',  ( -151.4692556286852891, -192.8130981290892692, 59.65701158161632378 ) ) ;
#3160 = CARTESIAN_POINT ( 'NONE',  ( 39.92123440845004723, 108.2604996726487627, 29.95742577749337343 ) ) ;
#3161 = CARTESIAN_POINT ( 'NONE',  ( 45.74753988029933538, 64.16518717409400097, 37.97664729208901946 ) ) ;
#3162 = CARTESIAN_POINT ( 'NONE',  ( 39.92123440845005433, 66.23445800887257917, 38.46393386101375711 ) ) ;
#3163 = CARTESIAN_POINT ( 'NONE',  ( -160.8964159109769696, -158.0438272943107165, 46.59394152635518083 ) ) ;
#3164 = CARTESIAN_POINT ( 'NONE',  ( -148.3790856849358306, -165.3891397928654499, 40.14644641866477315 ) ) ;
#3165 = CARTESIAN_POINT ( 'NONE',  ( -154.5594255724347761, -177.9630981290893033, 59.16757674456785310 ) ) ;
#3166 = SHAPE_REPRESENTATION_RELATIONSHIP ( 'NONE' , 'NONE' ,  #8609, #1649 ) ;
#3167 = CARTESIAN_POINT ( 'NONE',  ( -151.4692556286852891, -196.9891397928655010, 49.65701158161630957 ) ) ;
#3168 = CARTESIAN_POINT ( 'NONE',  ( 38.96631938032478359, 150.0844580088725593, 37.14960608071593384 ) ) ;
#3169 = CARTESIAN_POINT ( 'NONE',  ( 38.58424406990784661, 132.2297705074272756, 32.77220824515698183 ) ) ;
#3170 = CARTESIAN_POINT ( 'NONE',  ( 77.17837728419731036, 116.7372127726149245, 18.69201499742705153 ) ) ;
#3171 = CARTESIAN_POINT ( 'NONE',  ( 38.58424406990785371, 113.9651871740940123, 32.77220824515697473 ) ) ;
#3172 = CARTESIAN_POINT ( 'NONE',  ( -159.5594255724347761, -170.7891397928654840, 43.77915905869157598 ) ) ;
#3173 = PRODUCT_DEFINITION_FORMATION_WITH_SPECIFIED_SOURCE ( 'ANY', '', #15187, .NOT_KNOWN. ) ;
#3174 = CARTESIAN_POINT ( 'NONE',  ( 43.01140435219952707, 140.9604996726487514, 29.21067981925357060 ) ) ;
#3175 = CARTESIAN_POINT ( 'NONE',  ( 70.43474449472395804, 99.54920534645194152, 7.295875980836476593 ) ) ;
#3176 = CARTESIAN_POINT ( 'NONE',  ( 69.25106277675128297, 109.5764507715396832, -0.9149236002526208722 ) ) ;
#3177 = CARTESIAN_POINT ( 'NONE',  ( -141.4692556286852891, -186.9891397928654726, 49.65701158161630957 ) ) ;
#3178 = CARTESIAN_POINT ( 'NONE',  ( 40.27526882409969744, 95.92977050742732104, 30.44471234641812174 ) ) ;
#3179 = ORIENTED_EDGE ( 'NONE', *, *, #26, .F. ) ;
#3180 = CARTESIAN_POINT ( 'NONE',  ( 96.62434152388763664, 220.7958015105191976, -5.999999999999976019 ) ) ;
#3181 = ORIENTED_EDGE ( 'NONE', *, *, #12830, .F. ) ;
#3182 = CARTESIAN_POINT ( 'NONE',  ( 39.92123440845004723, 87.23445800887259338, 38.46393386101376421 ) ) ;
#3183 = CARTESIAN_POINT ( 'NONE',  ( 147.8787791192428074, -136.9891397928655010, 10.34298841838370642 ) ) ;
#3184 = VECTOR ( 'NONE', #9389, 1000.000000000000000 ) ;
#3185 = CARTESIAN_POINT ( 'NONE',  ( 39.92123440845004723, 136.1604996726487116, 38.46393386101376421 ) ) ;
#3187 = CARTESIAN_POINT ( 'NONE',  ( 27.89715912807487186, 143.6191053679247602, 4.279900468622926724 ) ) ;
#3186 = CARTESIAN_POINT ( 'NONE',  ( 43.01140435219951286, 92.36518717409398960, 29.55568802177586463 ) ) ;
#3188 = CARTESIAN_POINT ( 'NONE',  ( -156.1828648351502409, -155.3945647575687872, 41.49286807254280518 ) ) ;
#3189 = CARTESIAN_POINT ( 'NONE',  ( -160.8964159109769696, -167.0084106276440536, 52.72008163687743121 ) ) ;
#3190 = CARTESIAN_POINT ( 'NONE',  ( -143.8425227516148084, -192.0938272943107279, 44.11586579668791330 ) ) ;
#3192 = CARTESIAN_POINT ( 'NONE',  ( 48.01140435219951996, 70.13445800887255643, 35.83527830041809636 ) ) ;
#3191 = CARTESIAN_POINT ( 'NONE',  ( -161.4692556286853176, -178.5630981290893260, 49.65701158161630957 ) ) ;
#3193 = FACE_OUTER_BOUND ( 'NONE', #7898, .T. ) ;
#3194 = CARTESIAN_POINT ( 'NONE',  ( -141.4692556286852891, -177.2130981290892748, 52.90620854394536821 ) ) ;
#3195 = CARTESIAN_POINT ( 'NONE',  ( 48.01140435219951996, 115.4344580088725678, 32.58608133808903773 ) ) ;
#3196 = CARTESIAN_POINT ( 'NONE',  ( 40.27526882409969033, 60.56518717409398533, 37.97664729208901946 ) ) ;
#3197 = LINE ( 'NONE', #6738, #17161 ) ;
#3198 = CARTESIAN_POINT ( 'NONE',  ( 71.03835150376274044, 100.2492380157770526, 6.267546321443639989 ) ) ;
#3199 = CARTESIAN_POINT ( 'NONE',  ( 47.43856463449117911, 142.7651871740939669, 32.77220824515697473 ) ) ;
#3200 = CARTESIAN_POINT ( 'NONE',  ( -145.6429501568359797, -161.9438272943107222, 41.63779006702063867 ) ) ;
#3201 = CARTESIAN_POINT ( 'NONE',  ( -154.3824083646099439, -173.7584106276440536, 40.69124936498395328 ) ) ;
#3202 = ORIENTED_EDGE ( 'NONE', *, *, #14985, .T. ) ;
#3203 = CARTESIAN_POINT ( 'NONE',  ( 40.27526882409969744, 63.56518717409399954, 37.97664729208901235 ) ) ;
#3204 = CARTESIAN_POINT ( 'NONE',  ( -157.2955611005346270, -157.7084106276440423, 57.67623309621198047 ) ) ;
#3205 = CARTESIAN_POINT ( 'NONE',  ( 10.15219960346482431, 110.0225462658725490, 14.76332465322822074 ) ) ;
#3206 = CARTESIAN_POINT ( 'NONE',  ( 44.37947211624943833, 128.2151871740939839, 30.00020018409699318 ) ) ;
#3207 = EDGE_CURVE ( 'NONE', #8340, #4358, #8952, .T. ) ;
#3208 = CARTESIAN_POINT ( 'NONE',  ( 29.26409511065843105, 88.64202804534433255, -5.203872050689020590 ) ) ;
#3209 = VERTEX_POINT ( 'NONE', #18831 ) ;
#3210 = EDGE_LOOP ( 'NONE', ( #14662, #4234, #21319, #10321 ) ) ;
#3211 = FACE_OUTER_BOUND ( 'NONE', #21508, .T. ) ;
#3212 = EDGE_LOOP ( 'NONE', ( #10152, #12911, #16288, #16341 ) ) ;
#3213 = CARTESIAN_POINT ( 'NONE',  ( 41.64333658814960870, 156.9797705074273040, 38.42115945441014446 ) ) ;
#3214 = CARTESIAN_POINT ( 'NONE',  ( 40.27526882409969033, 65.92977050742732104, 30.44471234641811819 ) ) ;
#3216 = CARTESIAN_POINT ( 'NONE',  ( 66.10898071834657230, 103.7292514542787245, 6.347102411281516865 ) ) ;
#3215 = CARTESIAN_POINT ( 'NONE',  ( 41.64333658814960870, 123.7151871740940123, 38.42115945441014446 ) ) ;
#3217 =( BOUNDED_CURVE ( )  B_SPLINE_CURVE ( 2, ( #6620, #10143, #11563, #16629, #1759, #6500, #13219, #19957, #4842, #18292, #1539, #13335, #11670 ),
 .UNSPECIFIED., .F., .F. ) 
 B_SPLINE_CURVE_WITH_KNOTS ( ( 3, 2, 2, 2, 2, 2, 3 ),
 ( 0.1102941176470588203, 0.1117647058823529466, 0.1147058823529411714, 0.1176470588235294101, 0.1205882352941176489, 0.1235294117647058876, 0.1250000000000000000 ),
 .UNSPECIFIED. ) 
 CURVE ( )  GEOMETRIC_REPRESENTATION_ITEM ( )  RATIONAL_B_SPLINE_CURVE ( ( 0.9755282581475767101, 0.9755282581475765991, 1.000000000000000000, 0.9510565162951535312, 1.000000000000000000, 0.9510565162951535312, 1.000000000000000000, 0.9510565162951535312, 1.000000000000000000, 0.9510565162951535312, 1.000000000000000000, 0.9755282581475768211, 0.9755282581475768211 ) ) 
 REPRESENTATION_ITEM ( '' )  );
#3218 = CARTESIAN_POINT ( 'NONE',  ( 38.01140435219952707, 78.71049967264875136, 34.21067981925357060 ) ) ;
#3219 = DIRECTION ( 'NONE',  ( 1.000000000000000000, 0.000000000000000000, 0.000000000000000000 ) ) ;
#3220 = CARTESIAN_POINT ( 'NONE',  ( 39.92123440845005433, 144.2604996726487627, 29.95742577749336988 ) ) ;
#3221 = LINE ( 'NONE', #16433, #15274 ) ;
#3222 = CARTESIAN_POINT ( 'NONE',  ( 38.58424406990784661, 83.96518717409399812, 32.77220824515698183 ) ) ;
#3223 = CARTESIAN_POINT ( 'NONE',  ( 38.96631938032478359, 82.01049967264874851, 37.14960608071593384 ) ) ;
#3224 = CARTESIAN_POINT ( 'NONE',  ( -157.6495955161842062, -185.9391397928654612, 41.15050349809589392 ) ) ;
#3225 = ORIENTED_EDGE ( 'NONE', *, *, #13221, .F. ) ;
#3226 = CARTESIAN_POINT ( 'NONE',  ( 47.43856463449117200, 62.02977050742732246, 32.77220824515698183 ) ) ;
#3227 = CARTESIAN_POINT ( 'NONE',  ( -143.8425227516148084, -159.0938272943107279, 44.11586579668791330 ) ) ;
#3228 = CARTESIAN_POINT ( 'NONE',  ( 50.92548328124963319, 86.60151408976496157, 0.07716523989554470442 ) ) ;
#3229 = EDGE_CURVE ( 'NONE', #12336, #6852, #3737, .T. ) ;
#3230 = CARTESIAN_POINT ( 'NONE',  ( -159.0959885057557983, -188.4584106276440423, 44.11586579668791330 ) ) ;
#3231 = ORIENTED_EDGE ( 'NONE', *, *, #16655, .F. ) ;
#3232 = CARTESIAN_POINT ( 'NONE',  ( 45.74753988029933538, 154.1651871740939441, 37.97664729208901946 ) ) ;
#3233 = VECTOR ( 'NONE', #34, 999.9999999999998863 ) ;
#3234 = CARTESIAN_POINT ( 'NONE',  ( 43.01140435219951286, 106.4604996726487371, 39.21067981925356349 ) ) ;
#3235 = CARTESIAN_POINT ( 'NONE',  ( 39.42975644700377558, 114.6797705074273210, 36.81289934271958941 ) ) ;
#3236 = CARTESIAN_POINT ( 'NONE',  ( 73.40451243997107156, 135.6611253642151098, -1.946480675884423084 ) ) ;
#3237 = ORIENTED_EDGE ( 'NONE', *, *, #5860, .T. ) ;
#3238 = AXIS2_PLACEMENT_3D ( 'NONE', #19808, #9892, #3049 ) ;
#3239 = CARTESIAN_POINT ( 'NONE',  ( 16.16443657470430750, 128.5343009702184816, -4.486436360144259616 ) ) ;
#3240 = ORIENTED_EDGE ( 'NONE', *, *, #16105, .T. ) ;
#3241 = CARTESIAN_POINT ( 'NONE',  ( 39.42975644700377558, 114.6797705074273210, 36.81289934271958941 ) ) ;
#3242 = CARTESIAN_POINT ( 'NONE',  ( -101.1064508287285832, 10.96617311717548660, 4.000000000000021316 ) ) ;
#3243 = CARTESIAN_POINT ( 'NONE',  ( 44.37947211624943833, 152.2151871740940123, 30.00020018409699318 ) ) ;
#3244 = CARTESIAN_POINT ( 'NONE',  ( 53.88337135589062399, 152.3674195137575964, -9.803719146365084569 ) ) ;
#3245 = AXIS2_PLACEMENT_3D ( 'NONE', #14951, #21587, #3910 ) ;
#3246 = AXIS2_PLACEMENT_3D ( 'NONE', #1592, #6888, #8546 ) ;
#3247 = CARTESIAN_POINT ( 'NONE',  ( 42.21948215057684450, 107.1113394311928460, 29.21067981925356705 ) ) ;
#3248 = SURFACE_STYLE_USAGE ( .BOTH. , #6887 ) ;
#3249 = FACE_OUTER_BOUND ( 'NONE', #2020, .T. ) ;
#3250 = CARTESIAN_POINT ( 'NONE',  ( -148.3790856849358306, -178.5891397928654669, 59.16757674456786020 ) ) ;
#3251 = CARTESIAN_POINT ( 'NONE',  ( 39.92123440845005433, 89.33445800887257349, 29.95742577749336988 ) ) ;
#3252 = CARTESIAN_POINT ( 'NONE',  ( 47.05648932407426344, 131.5104996726487343, 31.27175355779120025 ) ) ;
#3253 = CARTESIAN_POINT ( 'NONE',  ( 44.55648932407425633, 77.81049967264873146, 29.45539723777780239 ) ) ;
#3254 = CIRCLE ( 'NONE', #21207, 3.000000000000000444 ) ;
#3255 = CARTESIAN_POINT ( 'NONE',  ( 44.37947211624943833, 92.47977050742731819, 30.00020018409699318 ) ) ;
#3256 = CARTESIAN_POINT ( 'NONE',  ( 18.01452421378985136, 106.6802099491036273, 21.62814552769798837 ) ) ;
#3257 = CARTESIAN_POINT ( 'NONE',  ( -154.3824083646099439, -187.2938272943107449, 58.62277379824867296 ) ) ;
#3258 = CARTESIAN_POINT ( 'NONE',  ( 38.58424406990785371, 83.96518717409399812, 32.77220824515697473 ) ) ;
#3259 = CARTESIAN_POINT ( 'NONE',  ( 42.21948215057684450, 84.03738109496899256, 29.21067981925356705 ) ) ;
#3260 = EDGE_LOOP ( 'NONE', ( #6641, #16425, #15413, #4890, #20873, #14634, #7629 ) ) ;
#3261 = FACE_OUTER_BOUND ( 'NONE', #9156, .T. ) ;
#3262 = CARTESIAN_POINT ( 'NONE',  ( 22.01597290215339697, 101.2010103422484519, -4.648787059867797389 ) ) ;
#3263 = PRODUCT_DEFINITION_SHAPE ( 'NONE', 'NONE',  #21827 ) ;
#3264 = EDGE_CURVE ( 'NONE', #2548, #5724, #3734, .T. ) ;
#3265 = CARTESIAN_POINT ( 'NONE',  ( 43.01140435219951286, 61.12977050742731677, 38.86567161673127657 ) ) ;
#3266 = VERTEX_POINT ( 'NONE', #11164 ) ;
#3267 = CARTESIAN_POINT ( 'NONE',  ( 38.58424406990784661, 141.2297705074273040, 32.77220824515698183 ) ) ;
#3268 = CARTESIAN_POINT ( 'NONE',  ( 46.59305225739526435, 97.57977050742731251, 36.81289934271958941 ) ) ;
#3269 = CARTESIAN_POINT ( 'NONE',  ( 47.05648932407426344, 110.5104996726487343, 31.27175355779120025 ) ) ;
#3270 = CARTESIAN_POINT ( 'NONE',  ( 45.74753988029933538, 67.16518717409401518, 37.97664729208901946 ) ) ;
#3271 = DIRECTION ( 'NONE',  ( 0.000000000000000000, 1.000000000000000000, 0.000000000000000000 ) ) ;
#3272 = CARTESIAN_POINT ( 'NONE',  ( -159.0959885057557983, -166.5938272943107563, 55.19815736654470584 ) ) ;
#3273 = CARTESIAN_POINT ( 'NONE',  ( 43.01140435219951996, 155.0344580088726048, 29.21067981925357060 ) ) ;
#3274 = CARTESIAN_POINT ( 'NONE',  ( -148.3790856849358306, -180.6630981290893203, 59.16757674456786020 ) ) ;
#3275 = DIRECTION ( 'NONE',  ( -1.000000000000000000, 0.000000000000000000, -2.437363037925170562E-16 ) ) ;
#3276 = EDGE_CURVE ( 'NONE', #8458, #14342, #14465, .T. ) ;
#3277 = CARTESIAN_POINT ( 'NONE',  ( 38.01140435219952707, 155.7844580088725763, 34.21067981925357060 ) ) ;
#3278 = CARTESIAN_POINT ( 'NONE',  ( 40.27526882409969033, 120.8297705074272983, 37.97664729208901946 ) ) ;
#3279 = CARTESIAN_POINT ( 'NONE',  ( 73.69864372527810303, 135.2613471474284097, 11.07306444099484466 ) ) ;
#3280 = LINE ( 'NONE', #12898, #5354 ) ;
#3281 = CARTESIAN_POINT ( 'NONE',  ( 45.74753988029934249, 113.0651871740940067, 30.44471234641812174 ) ) ;
#3282 = CARTESIAN_POINT ( 'NONE',  ( 0.000000000000000000, -37.13255853780189852, 30.00000000000000000 ) ) ;
#3283 = CARTESIAN_POINT ( 'NONE',  ( 147.5268905834513475, 193.0332408774651185, 14.00000000000001776 ) ) ;
#3284 = CARTESIAN_POINT ( 'NONE',  ( 61.89860894053757789, 148.3622700476249463, -1.513601781051955530 ) ) ;
#3285 = EDGE_CURVE ( 'NONE', #9423, #15135, #21427, .T. ) ;
#3286 = CARTESIAN_POINT ( 'NONE',  ( 50.21395344324809429, 147.1711500555979626, 4.203964687196366512 ) ) ;
#3287 = LINE ( 'NONE', #16720, #10407 ) ;
#3288 = CARTESIAN_POINT ( 'NONE',  ( 38.58424406990786082, 99.37977050742732388, 34.21067981925357060 ) ) ;
#3289 = ORIENTED_EDGE ( 'NONE', *, *, #9467, .T. ) ;
#3290 = EDGE_CURVE ( 'NONE', #19742, #18253, #917, .T. ) ;
#3291 = CIRCLE ( 'NONE', #15601, 10.00000000000003730 ) ;
#3292 = CARTESIAN_POINT ( 'NONE',  ( 138.2149183826930425, 102.3264679885537305, 4.000000000000021316 ) ) ;
#3293 = ORIENTED_EDGE ( 'NONE', *, *, #3630, .T. ) ;
#3294 = CARTESIAN_POINT ( 'NONE',  ( 39.92123440845004723, 83.33445800887255928, 29.95742577749337343 ) ) ;
#3295 = CARTESIAN_POINT ( 'NONE',  ( 43.01140435219951286, 87.53445800887257633, 39.21067981925356349 ) ) ;
#3296 = CARTESIAN_POINT ( 'NONE',  ( 47.05648932407426344, 143.5104996726487627, 31.27175355779120025 ) ) ;
#3298 = CARTESIAN_POINT ( 'NONE',  ( 21.19424684193554143, 137.6478987072957807, 3.922641511544080917 ) ) ;
#3297 = CARTESIAN_POINT ( 'NONE',  ( 44.37947211624943833, 100.0151871740939953, 38.42115945441014446 ) ) ;
#3299 = CARTESIAN_POINT ( 'NONE',  ( -151.4692556286852891, -170.9084106276440593, 39.74470866294723947 ) ) ;
#3300 = CARTESIAN_POINT ( 'NONE',  ( -148.5561028927606344, -194.7938272943107449, 40.69124936498395328 ) ) ;
#3302 = CARTESIAN_POINT ( 'NONE',  ( 47.05648932407426344, 70.58445800887257349, 31.27175355779120025 ) ) ;
#3301 = CARTESIAN_POINT ( 'NONE',  ( -161.4692556286852891, -166.4130981290892919, 52.90620854394536821 ) ) ;
#3303 = CARTESIAN_POINT ( 'NONE',  ( -151.4692556286852891, -189.8130981290892976, 59.65701158161632378 ) ) ;
#3304 = ADVANCED_FACE ( 'NONE', ( #16007, #13043, #19880, #9417 ), #4433, .F. ) ;
#3305 = CARTESIAN_POINT ( 'NONE',  ( -141.4692556286852891, -174.9891397928654726, 49.65701158161630957 ) ) ;
#3306 = CARTESIAN_POINT ( 'NONE',  ( 46.10157429594899270, 114.8344580088725877, 38.46393386101375711 ) ) ;
#3307 = CARTESIAN_POINT ( 'NONE',  ( 38.58424406990786082, 150.3797705074273097, 34.21067981925357060 ) ) ;
#3308 = CARTESIAN_POINT ( 'NONE',  ( 42.21948215057684450, 62.11133943119284595, 29.21067981925356705 ) ) ;
#3309 = CARTESIAN_POINT ( 'NONE',  ( 17.14282613681034917, 97.48634091255654255, 8.291567264837656381 ) ) ;
#3310 = CARTESIAN_POINT ( 'NONE',  ( 38.58424406990786082, 150.1151871740939896, 34.21067981925357060 ) ) ;
#3311 = CARTESIAN_POINT ( 'NONE',  ( -157.2955611005346270, -166.4438272943107506, 57.67623309621198047 ) ) ;
#3312 = CARTESIAN_POINT ( 'NONE',  ( -148.5561028927606344, -172.2584106276440536, 58.62277379824867296 ) ) ;
#3313 = EDGE_CURVE ( 'NONE', #15277, #4525, #17769, .T. ) ;
#3314 = ORIENTED_EDGE ( 'NONE', *, *, #21402, .T. ) ;
#3315 = CARTESIAN_POINT ( 'NONE',  ( 39.42975644700377558, 62.81518717409399954, 31.60846029578754468 ) ) ;
#3316 = CARTESIAN_POINT ( 'NONE',  ( -142.0420953463935803, -156.8084106276440366, 52.72008163687743831 ) ) ;
#3317 = CARTESIAN_POINT ( 'NONE',  ( 52.31916092102454741, 146.6125112339981627, 3.294994845742023948 ) ) ;
#3318 = CARTESIAN_POINT ( 'NONE',  ( 42.21948215057684450, 134.1113394311928175, 29.21067981925356705 ) ) ;
#3319 = CARTESIAN_POINT ( 'NONE',  ( 46.59305225739526435, 121.3151871740940067, 36.81289934271958941 ) ) ;
#3320 = ORIENTED_EDGE ( 'NONE', *, *, #2823, .F. ) ;
#3321 = ORIENTED_EDGE ( 'NONE', *, *, #8843, .T. ) ;
#3322 = CARTESIAN_POINT ( 'NONE',  ( 38.96631938032478359, 113.4844580088725792, 31.27175355779120025 ) ) ;
#3323 = ORIENTED_EDGE ( 'NONE', *, *, #1773, .F. ) ;
#3324 = CARTESIAN_POINT ( 'NONE',  ( 43.01140435219951286, 155.6297705074273097, 29.55568802177586107 ) ) ;
#3325 = CARTESIAN_POINT ( 'NONE',  ( 40.27526882409969033, 68.92977050742733525, 30.44471234641811819 ) ) ;
#3327 = CARTESIAN_POINT ( 'NONE',  ( 68.29827362630597065, 132.3882971431532383, 5.156253003121209488 ) ) ;
#3326 = CARTESIAN_POINT ( 'NONE',  ( 45.74753988029933538, 124.1651871740940152, 37.97664729208901946 ) ) ;
#3328 = CARTESIAN_POINT ( 'NONE',  ( 48.01140435219951996, 77.36049967264874283, 32.58608133808903773 ) ) ;
#3329 = CARTESIAN_POINT ( 'NONE',  ( 0.000000000000000000, -126.9891397928655010, 0.000000000000000000 ) ) ;
#3330 = EDGE_CURVE ( 'NONE', #12794, #19825, #7275, .T. ) ;
#3331 = CARTESIAN_POINT ( 'NONE',  ( 48.01140435219951996, 98.21049967264875136, 34.21067981925357060 ) ) ;
#3332 = FACE_OUTER_BOUND ( 'NONE', #19635, .T. ) ;
#3333 = CIRCLE ( 'NONE', #20241, 10.00000000000000888 ) ;
#3334 = CARTESIAN_POINT ( 'NONE',  ( 44.37947211624943833, 86.21518717409399812, 30.00020018409699318 ) ) ;
#3335 = CARTESIAN_POINT ( 'NONE',  ( 38.51811260612901577, 144.5002972345523631, 36.42795439419948877 ) ) ;
#3336 = DIRECTION ( 'NONE',  ( -0.4874675571821265319, -0.8731411001063289490, 0.000000000000000000 ) ) ;
#3337 = ORIENTED_EDGE ( 'NONE', *, *, #6526, .F. ) ;
#3338 = CARTESIAN_POINT ( 'NONE',  ( 46.59305225739526435, 68.17977050742732104, 31.60846029578754468 ) ) ;
#3339 = CARTESIAN_POINT ( 'NONE',  ( -145.6429501568359797, -187.1084106276440480, 57.67623309621198047 ) ) ;
#3340 = CARTESIAN_POINT ( 'NONE',  ( 28.65042173108665935, 151.0721679115347911, -4.641026357035400451 ) ) ;
#3341 = CARTESIAN_POINT ( 'NONE',  ( -148.5561028927606344, -175.2584106276440536, 58.62277379824867296 ) ) ;
#3342 = ORIENTED_EDGE ( 'NONE', *, *, #10504, .F. ) ;
#3343 = CARTESIAN_POINT ( 'NONE',  ( 43.01140435219951286, 153.8651871740939612, 38.86567161673127657 ) ) ;
#3344 = DIRECTION ( 'NONE',  ( 0.000000000000000000, 1.000000000000000000, 0.000000000000000000 ) ) ;
#3345 = CARTESIAN_POINT ( 'NONE',  ( 38.58424406990786082, 111.3797705074273239, 34.21067981925357060 ) ) ;
#3346 = CARTESIAN_POINT ( 'NONE',  ( 50.33192209904863290, 153.3481575868430014, -9.922832680162505525 ) ) ;
#3347 = ORIENTED_EDGE ( 'NONE', *, *, #4494, .T. ) ;
#3348 = ADVANCED_FACE ( 'NONE', ( #2789 ), #9531, .T. ) ;
#3349 = CARTESIAN_POINT ( 'NONE',  ( 34.72595348466361287, 146.8618156516888291, -3.415175568290148345 ) ) ;
#3350 =( BOUNDED_CURVE ( )  B_SPLINE_CURVE ( 2, ( #13006, #11020, #7940, #5836, #19294, #17843, #17730, #2636, #7730, #4395, #10920, #6157, #778 ),
 .UNSPECIFIED., .F., .F. ) 
 B_SPLINE_CURVE_WITH_KNOTS ( ( 3, 2, 2, 2, 2, 2, 3 ),
 ( 0.1607142857142856984, 0.1642857142857142849, 0.1714285714285714302, 0.1785714285714285754, 0.1857142857142857206, 0.1928571428571428659, 0.1964285714285714524 ),
 .UNSPECIFIED. ) 
 CURVE ( )  GEOMETRIC_REPRESENTATION_ITEM ( )  RATIONAL_B_SPLINE_CURVE ( ( 0.9755282581475768211, 0.9755282581475767101, 1.000000000000000000, 0.9510565162951535312, 1.000000000000000000, 0.9510565162951535312, 1.000000000000000000, 0.9510565162951535312, 1.000000000000000000, 0.9510565162951535312, 1.000000000000000000, 0.9755282581475765991, 0.9755282581475767101 ) ) 
 REPRESENTATION_ITEM ( '' )  );
#3351 = EDGE_LOOP ( 'NONE', ( #5084, #7985, #17552, #7309 ) ) ;
#3352 = CARTESIAN_POINT ( 'NONE',  ( 46.59305225739526435, 116.1797705074273210, 31.60846029578754468 ) ) ;
#3353 = CARTESIAN_POINT ( 'NONE',  ( -151.4692556286852891, -136.9891397928655010, -54.65701158161630246 ) ) ;
#3354 = CARTESIAN_POINT ( 'NONE',  ( 39.42975644700377558, 158.8151871740940067, 31.60846029578754468 ) ) ;
#3355 = ADVANCED_FACE ( 'NONE', ( #3010 ), #5985, .T. ) ;
#3356 = CARTESIAN_POINT ( 'NONE',  ( 76.20123706073158587, 111.5182621349952257, -8.137091297256032973 ) ) ;
#3357 = CARTESIAN_POINT ( 'NONE',  ( 46.10157429594899270, 81.83445800887258770, 38.46393386101375711 ) ) ;
#3358 = CARTESIAN_POINT ( 'NONE',  ( 162.3411339277076308, 184.7625696037766261, 272.0939500981630204 ) ) ;
#3359 = CARTESIAN_POINT ( 'NONE',  ( -148.3790856849358306, -175.5891397928654669, 59.16757674456786020 ) ) ;
#3360 = FACE_OUTER_BOUND ( 'NONE', #5933, .T. ) ;
#3361 = UNCERTAINTY_MEASURE_WITH_UNIT (LENGTH_MEASURE( 1.000000000000000082E-05 ), #1045, 'distance_accuracy_value', 'NONE');
#3362 = CARTESIAN_POINT ( 'NONE',  ( -154.5594255724347761, -193.8891397928654783, 59.16757674456785310 ) ) ;
#3363 = DIRECTION ( 'NONE',  ( 1.000000000000000000, 0.000000000000000000, 0.000000000000000000 ) ) ;
#3364 = APPLICATION_PROTOCOL_DEFINITION ( 'draft international standard', 'automotive_design', 1998, #1409 ) ;
#3365 = CARTESIAN_POINT ( 'NONE',  ( 38.96631938032478359, 99.08445800887258770, 37.14960608071593384 ) ) ;
#3366 = CARTESIAN_POINT ( 'NONE',  ( 44.37947211624943833, 91.27977050742731535, 38.42115945441014446 ) ) ;
#3367 = CARTESIAN_POINT ( 'NONE',  ( 57.86150831142030171, 95.93494642397840266, -0.2007220744356660869 ) ) ;
#3368 = CARTESIAN_POINT ( 'NONE',  ( -157.2955611005346270, -172.4438272943107506, 57.67623309621198047 ) ) ;
#3369 = EDGE_CURVE ( 'NONE', #13485, #120, #16125, .T. ) ;
#3370 = CARTESIAN_POINT ( 'NONE',  ( 47.43856463449117911, 91.76518717409399528, 32.77220824515697473 ) ) ;
#3371 = CYLINDRICAL_SURFACE ( 'NONE', #9726, 4.999999999999997335 ) ;
#3372 = ORIENTED_EDGE ( 'NONE', *, *, #5121, .T. ) ;
#3373 = FACE_BOUND ( 'NONE', #21625, .T. ) ;
#3374 = CARTESIAN_POINT ( 'NONE',  ( 74.27779736592162863, 105.9683817680885056, 13.05343286460986363 ) ) ;
#3375 = CARTESIAN_POINT ( 'NONE',  ( 15.79683473163509966, 126.9851207307152521, 3.446356185820485418 ) ) ;
#3376 = B_SPLINE_CURVE_WITH_KNOTS ( 'NONE', 3,
 ( #14477, #1367, #18231, #4897 ),
 .UNSPECIFIED., .F., .F.,
 ( 4, 4 ),
 ( 0.000000000000000000, 1.000000000000000000 ),
 .UNSPECIFIED. ) ;
#3377 = CARTESIAN_POINT ( 'NONE',  ( 41.64333658814960870, 59.77977050742731535, 30.00020018409699318 ) ) ;
#3378 = ORIENTED_EDGE ( 'NONE', *, *, #4559, .T. ) ;
#3379 = CARTESIAN_POINT ( 'NONE',  ( 47.43856463449118621, 148.8797705074273097, 34.21067981925357060 ) ) ;
#3380 = CARTESIAN_POINT ( 'NONE',  ( 46.59305225739526435, 94.57977050742731251, 36.81289934271958941 ) ) ;
#3381 = CARTESIAN_POINT ( 'NONE',  ( 43.80332655382220253, 155.8836182503284533, 29.21067981925356705 ) ) ;
#3382 = CARTESIAN_POINT ( 'NONE',  ( 44.55648932407425633, 104.8104996726487457, 29.45539723777780239 ) ) ;
#3383 = CARTESIAN_POINT ( 'NONE',  ( 39.42975644700377558, 63.41518717409400097, 36.81289934271958941 ) ) ;
#3384 = CARTESIAN_POINT ( 'NONE',  ( 163.1026836591718734, 192.4288937294299160, 34.00000000000001421 ) ) ;
#3385 = CARTESIAN_POINT ( 'NONE',  ( -157.2955611005345986, -161.3438272943107279, 41.63779006702063867 ) ) ;
#3386 = CARTESIAN_POINT ( 'NONE',  ( 38.96631938032478359, 123.0844580088725735, 37.14960608071593384 ) ) ;
#3387 = CARTESIAN_POINT ( 'NONE',  ( -145.2889157411863721, -171.5130981290893430, 58.16351966513671812 ) ) ;
#3388 =( NAMED_UNIT ( * ) PLANE_ANGLE_UNIT ( ) SI_UNIT ( $, .RADIAN. ) );
#3389 = CARTESIAN_POINT ( 'NONE',  ( -151.4692556286852891, -186.8130981290893260, 59.65701158161632378 ) ) ;
#3390 = CARTESIAN_POINT ( 'NONE',  ( 38.01140435219952707, 140.7844580088725763, 34.21067981925357060 ) ) ;
#3391 = EDGE_CURVE ( 'NONE', #13430, #16995, #21315, .T. ) ;
#3392 = CARTESIAN_POINT ( 'NONE',  ( 43.01140435219951286, 127.1297705074273381, 38.86567161673127657 ) ) ;
#3393 = CARTESIAN_POINT ( 'NONE',  ( 67.29571637068438861, 144.1510613573267108, 10.71565575886252297 ) ) ;
#3394 = LINE ( 'NONE', #14169, #19787 ) ;
#3395 = CARTESIAN_POINT ( 'NONE',  ( 38.58424406990786082, 117.1151871740940038, 34.21067981925357060 ) ) ;
#3396 = DIRECTION ( 'NONE',  ( -0.5010362705417047424, 0.000000000000000000, -0.8654262854811261008 ) ) ;
#3397 = CARTESIAN_POINT ( 'NONE',  ( -143.9637021292202235, -116.9891397928655010, 36.65701158161628825 ) ) ;
#3398 = CARTESIAN_POINT ( 'NONE',  ( 70.84804472268019992, 100.1183116193850964, 0.2719452077637916076 ) ) ;
#3399 = CARTESIAN_POINT ( 'NONE',  ( 18.57470074671828542, 105.8336742703428257, 1.585105279193314010 ) ) ;
#3400 = EDGE_CURVE ( 'NONE', #9553, #2626, #9376, .T. ) ;
#3401 = AXIS2_PLACEMENT_3D ( 'NONE', #9037, #19166, #15847 ) ;
#3402 = FACE_OUTER_BOUND ( 'NONE', #5526, .T. ) ;
#3403 = CARTESIAN_POINT ( 'NONE',  ( 40.27526882409969744, 90.82977050742731251, 37.97664729208901235 ) ) ;
#3404 = AXIS2_PLACEMENT_3D ( 'NONE', #14232, #14124, #7424 ) ;
#3405 = ADVANCED_FACE ( 'NONE', ( #4548 ), #6833, .T. ) ;
#3406 = ORIENTED_EDGE ( 'NONE', *, *, #16132, .F. ) ;
#3407 = CARTESIAN_POINT ( 'NONE',  ( 137.5268905834513191, 193.0332408774651185, 14.00000000000001776 ) ) ;
#3408 = EDGE_LOOP ( 'NONE', ( #14606, #4517, #12471, #2782 ) ) ;
#3409 = ADVANCED_FACE ( 'NONE', ( #11003 ), #15954, .F. ) ;
#3410 = CARTESIAN_POINT ( 'NONE',  ( 39.92123440845004723, 75.23445800887257917, 38.46393386101376421 ) ) ;
#3411 = CARTESIAN_POINT ( 'NONE',  ( 43.01140435219951996, 119.9070776186055838, 50.00000000000002842 ) ) ;
#3412 = CARTESIAN_POINT ( 'NONE',  ( 41.46631938032478359, 136.3104996726487457, 38.96596240072933170 ) ) ;
#3414 = CARTESIAN_POINT ( 'NONE',  ( 27.04509496028088478, 143.0549882411833380, 11.23409068567602098 ) ) ;
#3413 = CARTESIAN_POINT ( 'NONE',  ( 38.58424406990786082, 87.11518717409400381, 34.21067981925357060 ) ) ;
#3415 = ADVANCED_FACE ( 'NONE', ( #4274 ), #14303, .T. ) ;
#3416 = VECTOR ( 'NONE', #779, 1000.000000000000000 ) ;
#3417 = CARTESIAN_POINT ( 'NONE',  ( -160.8964159109769696, -161.1584106276440593, 49.65701158161630957 ) ) ;
#3418 = CARTESIAN_POINT ( 'NONE',  ( -160.8964159109769696, -191.0438272943107449, 46.59394152635518083 ) ) ;
#3419 = CARTESIAN_POINT ( 'NONE',  ( 43.01140435219951286, 113.0344580088725763, 29.21067981925356705 ) ) ;
#3420 = DIRECTION ( 'NONE',  ( -0.9393725726208708160, -0.3428981916074316239, 0.000000000000000000 ) ) ;
#3421 = CARTESIAN_POINT ( 'NONE',  ( 43.01140435219951996, 10.71049967264875491, 29.21067981925357060 ) ) ;
#3422 = CARTESIAN_POINT ( 'NONE',  ( 48.01140435219951996, 146.0604996726487457, 35.83527830041809636 ) ) ;
#3423 = VECTOR ( 'NONE', #10749, 1000.000000000000000 ) ;
#3424 = CARTESIAN_POINT ( 'NONE',  ( 45.74753988029933538, 149.3297705074273267, 30.44471234641811819 ) ) ;
#3425 = CARTESIAN_POINT ( 'NONE',  ( 43.01140435219951996, 10.71049967264875491, 34.21067981925357060 ) ) ;
#3426 = CARTESIAN_POINT ( 'NONE',  ( 35.69068542950036260, 86.46542255174357194, 7.577194441455407770 ) ) ;
#3427 = CARTESIAN_POINT ( 'NONE',  ( 41.64333658814960870, 147.7151871740940123, 38.42115945441014446 ) ) ;
#3428 = CARTESIAN_POINT ( 'NONE',  ( -160.8964159109769696, -160.7438272943107052, 52.72008163687743121 ) ) ;
#3429 = CARTESIAN_POINT ( 'NONE',  ( -148.5561028927606344, -174.0584106276440366, 40.69124936498395328 ) ) ;
#3430 = EDGE_LOOP ( 'NONE', ( #21340, #5954, #2243, #18078 ) ) ;
#3431 = CARTESIAN_POINT ( 'NONE',  ( 47.43856463449117911, 64.46518717409399812, 35.64915139335015937 ) ) ;
#3432 = CARTESIAN_POINT ( 'NONE',  ( -154.3824083646099439, -163.5584106276440366, 58.62277379824867296 ) ) ;
#3433 = CARTESIAN_POINT ( 'NONE',  ( 70.48772827241290884, 113.2068808858050630, -2.062176545857650201 ) ) ;
#3434 = DIRECTION ( 'NONE',  ( -1.000000000000000000, 0.000000000000000000, 0.000000000000000000 ) ) ;
#3435 = CARTESIAN_POINT ( 'NONE',  ( 38.58424406990786082, 123.1151871740940038, 34.21067981925357060 ) ) ;
#3436 = VECTOR ( 'NONE', #13943, 1000.000000000000000 ) ;
#3437 = CARTESIAN_POINT ( 'NONE',  ( 39.92123440845005433, 114.2344580088725650, 38.46393386101375711 ) ) ;
#3438 = ORIENTED_EDGE ( 'NONE', *, *, #5810, .F. ) ;
#3439 = CARTESIAN_POINT ( 'NONE',  ( 47.05648932407426344, 99.98445800887257917, 37.14960608071593384 ) ) ;
#3440 = CARTESIAN_POINT ( 'NONE',  ( 38.58424406990786082, 159.3797705074273381, 34.21067981925357060 ) ) ;
#3441 = CARTESIAN_POINT ( 'NONE',  ( 38.58424406990784661, 66.22977050742728977, 32.77220824515698183 ) ) ;
#3443 = CARTESIAN_POINT ( 'NONE',  ( 69.85845278386915425, 111.2786852186620621, 13.01367670771671747 ) ) ;
#3442 = CARTESIAN_POINT ( 'NONE',  ( 40.27526882409969033, 128.6651871740940010, 30.44471234641811819 ) ) ;
#3444 = EDGE_CURVE ( 'NONE', #20510, #12850, #16759, .T. ) ;
#3445 = AXIS2_PLACEMENT_3D ( 'NONE', #18461, #269, #3363 ) ;
#3446 = CARTESIAN_POINT ( 'NONE',  ( 39.92123440845004723, 81.26049967264872009, 29.95742577749337343 ) ) ;
#3447 = CYLINDRICAL_SURFACE ( 'NONE', #12876, 10.00000000000000888 ) ;
#3448 = FACE_OUTER_BOUND ( 'NONE', #15721, .T. ) ;
#3449 = CARTESIAN_POINT ( 'NONE',  ( 41.46631938032478359, 139.3104996726487457, 38.96596240072933170 ) ) ;
#3450 = CARTESIAN_POINT ( 'NONE',  ( 46.59305225739526435, 76.31518717409399244, 36.81289934271958941 ) ) ;
#3451 = CARTESIAN_POINT ( 'NONE',  ( 43.01140435219951286, 104.0344580088725763, 29.21067981925356705 ) ) ;
#3452 = VECTOR ( 'NONE', #8325, 1000.000000000000000 ) ;
#3453 = CARTESIAN_POINT ( 'NONE',  ( 147.5268905834513475, 193.0332408774651185, 4.000000000000021316 ) ) ;
#3454 = ORIENTED_EDGE ( 'NONE', *, *, #5441, .T. ) ;
#3455 = CARTESIAN_POINT ( 'NONE',  ( 44.37947211624943833, 70.27977050742731535, 38.42115945441014446 ) ) ;
#3456 = CARTESIAN_POINT ( 'NONE',  ( -151.4692556286852891, -188.9084106276440593, 39.74470866294723947 ) ) ;
#3457 = CARTESIAN_POINT ( 'NONE',  ( 12.61881386508366809, 104.1535352963828984, 15.55354899318430739 ) ) ;
#3458 = CARTESIAN_POINT ( 'NONE',  ( -142.0420953463935803, -177.5084106276440536, 46.59394152635518793 ) ) ;
#3459 = EDGE_LOOP ( 'NONE', ( #7718, #4157, #7317, #15466 ) ) ;
#3460 = CARTESIAN_POINT ( 'NONE',  ( 38.58424406990786082, 153.1151871740939896, 34.21067981925357060 ) ) ;
#3461 = DIRECTION ( 'NONE',  ( 1.000000000000000000, 0.000000000000000000, 0.000000000000000000 ) ) ;
#3462 = CARTESIAN_POINT ( 'NONE',  ( 46.59305225739526435, 110.1797705074273210, 31.60846029578754468 ) ) ;
#3463 = CARTESIAN_POINT ( 'NONE',  ( 69.83118287335672392, 141.1824132108841638, 4.838974892866481525 ) ) ;
#3464 = CIRCLE ( 'NONE', #2394, 10.00000000000000888 ) ;
#3465 = VERTEX_POINT ( 'NONE', #15747 ) ;
#3466 = EDGE_CURVE ( 'NONE', #9506, #10827, #4066, .T. ) ;
#3467 = EDGE_CURVE ( 'NONE', #5871, #8301, #1993, .T. ) ;
#3468 = ORIENTED_EDGE ( 'NONE', *, *, #8693, .F. ) ;
#3469 = CARTESIAN_POINT ( 'NONE',  ( 44.37947211624943833, 86.47977050742731819, 30.00020018409699318 ) ) ;
#3470 = CARTESIAN_POINT ( 'NONE',  ( 41.64333658814960870, 156.7151871740939839, 38.42115945441014446 ) ) ;
#3471 = CARTESIAN_POINT ( 'NONE',  ( 59.50342836137831171, 89.99885106877826502, 7.772197353298202493 ) ) ;
#3472 = CARTESIAN_POINT ( 'NONE',  ( 44.55648932407425633, 81.68445800887258201, 38.96596240072933170 ) ) ;
#3473 = DIRECTION ( 'NONE',  ( 0.7071067811865456854, 0.000000000000000000, 0.7071067811865493491 ) ) ;
#3474 = CARTESIAN_POINT ( 'NONE',  ( -148.3790856849358306, -184.5891397928654669, 59.16757674456786020 ) ) ;
#3475 = CARTESIAN_POINT ( 'NONE',  ( 139.9279279298906147, 262.8829071470229906, 4.000000000000021316 ) ) ;
#3476 = CARTESIAN_POINT ( 'NONE',  ( 144.5586921005913439, 133.1239846058259388, -19.99999999999999645 ) ) ;
#3477 = CARTESIAN_POINT ( 'NONE',  ( 46.10157429594899270, 92.66049967264873999, 29.95742577749336988 ) ) ;
#3478 = ITEM_DEFINED_TRANSFORMATION ( 'NONE', 'NONE', #2118,  #12657 ) ;
#3479 = CARTESIAN_POINT ( 'NONE',  ( 43.01140435219951286, 98.03445800887257633, 29.21067981925356705 ) ) ;
#3480 = CARTESIAN_POINT ( 'NONE',  ( 39.42975644700377558, 99.07977050742732672, 31.60846029578754468 ) ) ;
#3481 = CARTESIAN_POINT ( 'NONE',  ( 32.38101408406643600, 93.78751416920769657, -6.153149741203968404 ) ) ;
#3482 = CARTESIAN_POINT ( 'NONE',  ( -154.3824083646099439, -173.4938272943107336, 40.69124936498395328 ) ) ;
#3483 = CARTESIAN_POINT ( 'NONE',  ( 41.64333658814960870, 83.51518717409400949, 30.00020018409699318 ) ) ;
#3484 = LINE ( 'NONE', #12162, #3741 ) ;
#3485 = ORIENTED_EDGE ( 'NONE', *, *, #21498, .T. ) ;
#3486 = DIRECTION ( 'NONE',  ( 0.000000000000000000, 0.000000000000000000, 1.000000000000000000 ) ) ;
#3487 = CARTESIAN_POINT ( 'NONE',  ( 77.07719282571002850, 116.5297446719512209, 12.69640610750513865 ) ) ;
#3488 =( BOUNDED_CURVE ( )  B_SPLINE_CURVE ( 2, ( #8382, #16845, #2969, #9708, #5069, #15091, #1319, #13336, #6736, #21388, #18406, #13443, #4728 ),
 .UNSPECIFIED., .F., .T. ) 
 B_SPLINE_CURVE_WITH_KNOTS ( ( 3, 2, 2, 2, 2, 2, 3 ),
 ( 0.7720588235294117974, 0.7735294117647059098, 0.7764705882352941346, 0.7794117647058823595, 0.7823529411764705843, 0.7852941176470588092, 0.7867647058823529216 ),
 .UNSPECIFIED. ) 
 CURVE ( )  GEOMETRIC_REPRESENTATION_ITEM ( )  RATIONAL_B_SPLINE_CURVE ( ( 0.9755282581475768211, 0.9755282581475768211, 1.000000000000000000, 0.9510565162951535312, 1.000000000000000000, 0.9510565162951535312, 1.000000000000000000, 0.9510565162951535312, 1.000000000000000000, 0.9510565162951535312, 1.000000000000000000, 0.9755282581475768211, 0.9755282581475768211 ) ) 
 REPRESENTATION_ITEM ( '' )  );
#3489 = CARTESIAN_POINT ( 'NONE',  ( 39.42975644700377558, 141.6797705074273210, 36.81289934271958941 ) ) ;
#3490 = CARTESIAN_POINT ( 'NONE',  ( 17.65293208513390866, 132.0582047407114885, -3.339186312533837242 ) ) ;
#3491 = EDGE_CURVE ( 'NONE', #1853, #4221, #21002, .T. ) ;
#3492 = CARTESIAN_POINT ( 'NONE',  ( 41.46631938032478359, 119.1844580088725962, 29.45539723777780239 ) ) ;
#3493 = ORIENTED_EDGE ( 'NONE', *, *, #5154, .F. ) ;
#3494 = CARTESIAN_POINT ( 'NONE',  ( 40.27526882409969033, 141.8297705074273267, 37.97664729208901946 ) ) ;
#3495 = FACE_OUTER_BOUND ( 'NONE', #12, .T. ) ;
#3496 = VECTOR ( 'NONE', #14530, 1000.000000000000000 ) ;
#3497 = CARTESIAN_POINT ( 'NONE',  ( 129.2454342010813662, 193.1635054290503319, -29.99999999999997868 ) ) ;
#3498 = CARTESIAN_POINT ( 'NONE',  ( -151.4692556286852607, -157.7391397928654726, 59.65701158161632378 ) ) ;
#3499 = CARTESIAN_POINT ( 'NONE',  ( -143.8425227516148084, -156.0938272943107279, 44.11586579668791330 ) ) ;
#3500 = CARTESIAN_POINT ( 'NONE',  ( 43.01140435219951996, 10.71049967264875491, 39.21067981925356349 ) ) ;
#3501 = CARTESIAN_POINT ( 'NONE',  ( -154.5594255724347761, -165.9630981290893033, 59.16757674456785310 ) ) ;
#3502 =( LENGTH_UNIT ( ) NAMED_UNIT ( * ) SI_UNIT ( .MILLI., .METRE. ) );
#3503 = CARTESIAN_POINT ( 'NONE',  ( 41.46631938032478359, 147.3844580088725991, 38.96596240072933170 ) ) ;
#3504 = CARTESIAN_POINT ( 'NONE',  ( 41.64333658814960870, 123.9797705074273324, 38.42115945441014446 ) ) ;
#3505 = CARTESIAN_POINT ( 'NONE',  ( 9.955767346236717330, 110.6995739201198887, 21.78706596723887756 ) ) ;
#3506 = CARTESIAN_POINT ( 'NONE',  ( -149.8854112254399240, -184.6622583705452030, 59.65701158161632378 ) ) ;
#3507 = CARTESIAN_POINT ( 'NONE',  ( 45.74753988029934249, 116.0651871740939924, 30.44471234641812174 ) ) ;
#3508 = CARTESIAN_POINT ( 'NONE',  ( 147.8787791192428074, -126.9891397928655010, 10.34298841838370642 ) ) ;
#3509 = CARTESIAN_POINT ( 'NONE',  ( 41.12929731208597417, 154.0090796829547912, -2.227802639778228233 ) ) ;
#3510 = CARTESIAN_POINT ( 'NONE',  ( 70.21798013780751546, 127.3226622636268672, -1.629293503064584536 ) ) ;
#3511 = CARTESIAN_POINT ( 'NONE',  ( -149.8854112254399524, -185.3899795514095388, 39.65701158161630246 ) ) ;
#3512 = VECTOR ( 'NONE', #12725, 1000.000000000000000 ) ;
#3513 = CARTESIAN_POINT ( 'NONE',  ( 46.59305225739526435, 83.17977050742732104, 31.60846029578754468 ) ) ;
#3514 = ORIENTED_EDGE ( 'NONE', *, *, #12179, .F. ) ;
#3515 = CARTESIAN_POINT ( 'NONE',  ( -145.2889157411863437, -168.5130981290892578, 58.16351966513671812 ) ) ;
#3516 = CARTESIAN_POINT ( 'NONE',  ( 48.01140435219951996, 70.28445800887257633, 34.21067981925357060 ) ) ;
#3517 = CARTESIAN_POINT ( 'NONE',  ( 38.01140435219952707, 86.63445800887257064, 32.58608133808903773 ) ) ;
#3518 = CARTESIAN_POINT ( 'NONE',  ( 38.96631938032478359, 126.4104996726487542, 31.27175355779120025 ) ) ;
#3520 = CARTESIAN_POINT ( 'NONE',  ( 15.69291839309778958, 99.40984958608130739, -11.63272432674803802 ) ) ;
#3519 = CARTESIAN_POINT ( 'NONE',  ( 45.74753988029933538, 83.06518717409400665, 30.44471234641811819 ) ) ;
#3521 = CARTESIAN_POINT ( 'NONE',  ( -142.0420953463935803, -162.8084106276440650, 52.72008163687743831 ) ) ;
#3522 = CARTESIAN_POINT ( 'NONE',  ( -148.5561028927606344, -179.7938272943107449, 40.69124936498395328 ) ) ;
#3523 = CARTESIAN_POINT ( 'NONE',  ( 42.21948215057684450, 117.4575765865523067, 39.21067981925355639 ) ) ;
#3524 = FACE_OUTER_BOUND ( 'NONE', #7367, .T. ) ;
#3525 = CARTESIAN_POINT ( 'NONE',  ( 43.01140435219951286, 62.03445800887256922, 29.21067981925356705 ) ) ;
#3526 = CARTESIAN_POINT ( 'NONE',  ( 47.05648932407426344, 68.51049967264874851, 31.27175355779120025 ) ) ;
#3527 = CARTESIAN_POINT ( 'NONE',  ( -153.0531000319307111, -174.1622583705452314, 39.65701158161631668 ) ) ;
#3528 = CARTESIAN_POINT ( 'NONE',  ( 39.42975644700377558, 156.0797705074273267, 31.60846029578754468 ) ) ;
#3529 = CARTESIAN_POINT ( 'NONE',  ( 38.01140435219952707, 62.78445800887258343, 34.21067981925357060 ) ) ;
#3530 = CARTESIAN_POINT ( 'NONE',  ( 18.14018356548558941, 143.3940520581896862, 16.92415443696469879 ) ) ;
#3531 = CARTESIAN_POINT ( 'NONE',  ( 39.42975644700377558, 146.8151871740940067, 31.60846029578754468 ) ) ;
#3532 = CARTESIAN_POINT ( 'NONE',  ( 43.01140435219951996, 10.71049967264875491, 34.21067981925357060 ) ) ;
#3533 = CARTESIAN_POINT ( 'NONE',  ( -159.0959885057557983, -176.4584106276440707, 44.11586579668791330 ) ) ;
#3534 = CARTESIAN_POINT ( 'NONE',  ( 39.42975644700377558, 60.41518717409400097, 36.81289934271958941 ) ) ;
#3535 = CARTESIAN_POINT ( 'NONE',  ( -160.8964159109769696, -161.0084106276440252, 52.72008163687743121 ) ) ;
#3536 = CARTESIAN_POINT ( 'NONE',  ( 62.56935518920172967, 140.3353681171158200, 3.771274953561639887 ) ) ;
#3537 = DIRECTION ( 'NONE',  ( 0.000000000000000000, 1.000000000000000000, 0.000000000000000000 ) ) ;
#3538 = CARTESIAN_POINT ( 'NONE',  ( 43.01140435219951286, 126.8651871740940180, 38.86567161673127657 ) ) ;
#3539 = ORIENTED_EDGE ( 'NONE', *, *, #4151, .F. ) ;
#3540 = ORIENTED_EDGE ( 'NONE', *, *, #18228, .F. ) ;
#3541 = EDGE_CURVE ( 'NONE', #9751, #9805, #11486, .T. ) ;
#3542 = EDGE_LOOP ( 'NONE', ( #16227, #19650, #5450, #16336 ) ) ;
#3543 = CARTESIAN_POINT ( 'NONE',  ( 38.01140435219951996, 104.9344580088725820, 35.83527830041810347 ) ) ;
#3544 = CARTESIAN_POINT ( 'NONE',  ( 43.01140435219951286, 137.9604996726487514, 29.21067981925356705 ) ) ;
#3545 = CARTESIAN_POINT ( 'NONE',  ( 44.37947211624943833, 62.47977050742731109, 30.00020018409699318 ) ) ;
#3547 = CARTESIAN_POINT ( 'NONE',  ( 71.06985403747866314, 121.7623127629220932, -14.41049859375789666 ) ) ;
#3546 = CARTESIAN_POINT ( 'NONE',  ( 47.43856463449118621, 112.6151871740939896, 34.21067981925357060 ) ) ;
#3548 = CARTESIAN_POINT ( 'NONE',  ( 43.01140435219951286, 83.96049967264873715, 28.95336869806222779 ) ) ;
#3549 = CARTESIAN_POINT ( 'NONE',  ( 48.01140435219951996, 148.2844580088725763, 34.21067981925357060 ) ) ;
#3550 = LINE ( 'NONE', #6760, #19506 ) ;
#3551 = CARTESIAN_POINT ( 'NONE',  ( -161.4692556286852891, -190.7130981290893033, 46.40781461928724383 ) ) ;
#3552 = CARTESIAN_POINT ( 'NONE',  ( 43.01140435219951286, 81.86518717409398960, 38.86567161673127657 ) ) ;
#3553 = PRODUCT_DEFINITION_CONTEXT ( 'detailed design', #11668, 'design' ) ;
#3554 = CARTESIAN_POINT ( 'NONE',  ( 38.04343743846316528, 144.4085798130015803, 34.86469163422182049 ) ) ;
#3555 = CARTESIAN_POINT ( 'NONE',  ( 38.01140435219951996, 125.6344580088725706, 32.58608133808903773 ) ) ;
#3556 = DIRECTION ( 'NONE',  ( -0.000000000000000000, 1.000000000000000000, -0.000000000000000000 ) ) ;
#3557 = EDGE_CURVE ( 'NONE', #4126, #19197, #17936, .T. ) ;
#3558 = ORIENTED_EDGE ( 'NONE', *, *, #3290, .F. ) ;
#3559 = CARTESIAN_POINT ( 'NONE',  ( -142.0420953463936087, -189.6584106276440593, 49.65701158161630957 ) ) ;
#3560 = CARTESIAN_POINT ( 'NONE',  ( 28.07864021081662287, 89.10199518432737875, 14.83897397183228861 ) ) ;
#3561 = CARTESIAN_POINT ( 'NONE',  ( -142.0420953463935803, -180.8084106276440366, 52.72008163687743831 ) ) ;
#3562 = VERTEX_POINT ( 'NONE', #5816 ) ;
#3563 = CARTESIAN_POINT ( 'NONE',  ( 39.42975644700377558, 153.4151871740940010, 36.81289934271958941 ) ) ;
#3564 = EDGE_CURVE ( 'NONE', #1573, #10861, #4803, .T. ) ;
#3565 = LINE ( 'NONE', #567, #6404 ) ;
#3566 = EDGE_CURVE ( 'NONE', #5132, #8905, #20825, .T. ) ;
#3567 = CARTESIAN_POINT ( 'NONE',  ( 40.27526882409969744, 114.8297705074273267, 37.97664729208901235 ) ) ;
#3568 = CARTESIAN_POINT ( 'NONE',  ( 63.41425016244589585, 92.41789933959738335, 6.624947895572852019 ) ) ;
#3569 = ORIENTED_EDGE ( 'NONE', *, *, #6191, .F. ) ;
#3570 = VERTEX_POINT ( 'NONE', #12547 ) ;
#3571 = CARTESIAN_POINT ( 'NONE',  ( 47.43856463449117200, 110.0297705074273296, 32.77220824515698183 ) ) ;
#3572 = CARTESIAN_POINT ( 'NONE',  ( 38.01140435219952707, 158.6344580088725706, 32.58608133808903773 ) ) ;
#3573 = LINE ( 'NONE', #10298, #21348 ) ;
#3574 = CARTESIAN_POINT ( 'NONE',  ( 47.43856463449117200, 142.4651871740940123, 35.64915139335016647 ) ) ;
#3575 = CARTESIAN_POINT ( 'NONE',  ( 20.88913110926514705, 146.0313881486468119, 3.053432864643822686 ) ) ;
#3576 = FACE_BOUND ( 'NONE', #8312, .T. ) ;
#3577 = FACE_OUTER_BOUND ( 'NONE', #19092, .T. ) ;
#3578 = CARTESIAN_POINT ( 'NONE',  ( -159.5594255724347761, -182.1891397928654612, 55.53486410454104316 ) ) ;
#3579 = CARTESIAN_POINT ( 'NONE',  ( 48.01140435219951996, 101.3604996726487286, 32.58608133808903773 ) ) ;
#3580 = UNCERTAINTY_MEASURE_WITH_UNIT (LENGTH_MEASURE( 1.000000000000000082E-05 ), #3502, 'distance_accuracy_value', 'NONE');
#3581 = CARTESIAN_POINT ( 'NONE',  ( -161.4692556286852891, -194.6391397928654783, 46.40781461928724383 ) ) ;
#3582 = CARTESIAN_POINT ( 'NONE',  ( 44.55648932407425633, 96.68445800887258201, 38.96596240072933170 ) ) ;
#3583 = CARTESIAN_POINT ( 'NONE',  ( 41.64333658814960870, 98.77977050742731535, 30.00020018409699318 ) ) ;
#3584 = CARTESIAN_POINT ( 'NONE',  ( 16.33471683235446292, 110.7640000046674089, -5.200637885961103102 ) ) ;
#3585 = CARTESIAN_POINT ( 'NONE',  ( -143.8425227516148084, -177.6938272943107506, 55.19815736654470584 ) ) ;
#3586 = CARTESIAN_POINT ( 'NONE',  ( 41.64333658814960870, 80.51518717409400949, 30.00020018409699318 ) ) ;
#3587 = LINE ( 'NONE', #17017, #10630 ) ;
#3588 = CARTESIAN_POINT ( 'NONE',  ( -151.4692556286852607, -159.2391397928654726, 39.65701158161629536 ) ) ;
#3589 = ORIENTED_EDGE ( 'NONE', *, *, #18909, .T. ) ;
#3590 = CARTESIAN_POINT ( 'NONE',  ( -56.84366818088135176, 789.5005544000622422, -19.99999999999997868 ) ) ;
#3591 = EDGE_CURVE ( 'NONE', #4466, #7553, #14300, .T. ) ;
#3592 = CYLINDRICAL_SURFACE ( 'NONE', #10289, 4.999999999999997335 ) ;
#3593 = CARTESIAN_POINT ( 'NONE',  ( 65.16383128666855384, 137.2272505635282585, -1.077070130972596962 ) ) ;
#3594 = ORIENTED_EDGE ( 'NONE', *, *, #16609, .F. ) ;
#3595 = LINE ( 'NONE', #21789, #10796 ) ;
#3596 = VERTEX_POINT ( 'NONE', #9254 ) ;
#3597 = CARTESIAN_POINT ( 'NONE',  ( 40.27526882409969033, 138.8297705074272983, 37.97664729208901946 ) ) ;
#3598 = CIRCLE ( 'NONE', #12744, 10.00000000000003730 ) ;
#3599 = VECTOR ( 'NONE', #3344, 1000.000000000000000 ) ;
#3600 = CARTESIAN_POINT ( 'NONE',  ( 41.64333658814960870, 98.77977050742731535, 30.00020018409699318 ) ) ;
#3601 = CARTESIAN_POINT ( 'NONE',  ( 38.01140435219952707, 141.5604996726487457, 32.58608133808903773 ) ) ;
#3602 = EDGE_CURVE ( 'NONE', #14339, #10720, #6710, .T. ) ;
#3603 = AXIS2_PLACEMENT_3D ( 'NONE', #9604, #13419, #11757 ) ;
#3604 = DIRECTION ( 'NONE',  ( -0.3428981916074316239, 0.9393725726208708160, 0.000000000000000000 ) ) ;
#3605 = FACE_BOUND ( 'NONE', #4278, .T. ) ;
#3606 = LINE ( 'NONE', #20464, #19004 ) ;
#3607 = CARTESIAN_POINT ( 'NONE',  ( -148.3790856849358306, -173.4630981290893033, 40.14644641866477315 ) ) ;
#3608 = LINE ( 'NONE', #6915, #13566 ) ;
#3609 = CARTESIAN_POINT ( 'NONE',  ( -157.6495955161842062, -166.1130981290892521, 58.16351966513671812 ) ) ;
#3610 = CARTESIAN_POINT ( 'NONE',  ( 0.000000000000000000, 0.000000000000000000, 0.000000000000000000 ) ) ;
#3611 = CARTESIAN_POINT ( 'NONE',  ( 48.01140435219951996, 145.4344580088725820, 32.58608133808903773 ) ) ;
#3612 = CARTESIAN_POINT ( 'NONE',  ( 47.43856463449117200, 128.0297705074273154, 32.77220824515698183 ) ) ;
#3613 =( BOUNDED_CURVE ( )  B_SPLINE_CURVE ( 2, ( #9155, #7068, #9044, #20511, #15856, #5398, #10483, #13987, #12116, #7395, #20724, #545, #12335 ),
 .UNSPECIFIED., .F., .F. ) 
 B_SPLINE_CURVE_WITH_KNOTS ( ( 3, 2, 2, 2, 2, 2, 3 ),
 ( 0.3750000000000000000, 0.3785714285714285587, 0.3857142857142857317, 0.3928571428571428492, 0.4000000000000000222, 0.4071428571428571397, 0.4107142857142857539 ),
 .UNSPECIFIED. ) 
 CURVE ( )  GEOMETRIC_REPRESENTATION_ITEM ( )  RATIONAL_B_SPLINE_CURVE ( ( 0.9755282581475768211, 0.9755282581475768211, 1.000000000000000000, 0.9510565162951535312, 1.000000000000000000, 0.9510565162951535312, 1.000000000000000000, 0.9510565162951535312, 1.000000000000000000, 0.9510565162951535312, 1.000000000000000000, 0.9755282581475765991, 0.9755282581475768211 ) ) 
 REPRESENTATION_ITEM ( '' )  );
#3614 = CARTESIAN_POINT ( 'NONE',  ( 51.76721073900363734, 146.7980033588722506, -3.728880589165500137 ) ) ;
#3615 = CARTESIAN_POINT ( 'NONE',  ( -151.4692556286852891, -183.2391397928654726, 39.65701158161629536 ) ) ;
#3616 = CARTESIAN_POINT ( 'NONE',  ( 44.37947211624943833, 107.2151871740940123, 30.00020018409699318 ) ) ;
#3617 = LINE ( 'NONE', #304, #10490 ) ;
#3618 = CARTESIAN_POINT ( 'NONE',  ( 51.60797029699607918, 86.77139250312444574, -6.946567135388369785 ) ) ;
#3619 = CARTESIAN_POINT ( 'NONE',  ( 43.64334309031418968, 148.0990856179656419, -3.057864931601543823 ) ) ;
#3620 = CARTESIAN_POINT ( 'NONE',  ( -166.4803626276155626, -126.9891397928655010, 49.65701158161629536 ) ) ;
#3621 = CARTESIAN_POINT ( 'NONE',  ( 47.43856463449118621, 88.87977050742732388, 34.21067981925357060 ) ) ;
#3622 = VERTEX_POINT ( 'NONE', #19593 ) ;
#3623 = CARTESIAN_POINT ( 'NONE',  ( 43.01140435219951286, 144.5344580088726048, 39.21067981925356349 ) ) ;
#3624 = CARTESIAN_POINT ( 'NONE',  ( 43.01140435219951286, 72.53445800887259054, 39.46799094044489209 ) ) ;
#3625 = CARTESIAN_POINT ( 'NONE',  ( 38.96631938032478359, 87.08445800887258770, 37.14960608071593384 ) ) ;
#3626 = CARTESIAN_POINT ( 'NONE',  ( 47.05648932407426344, 130.9104996726487684, 37.14960608071593384 ) ) ;
#3628 = CARTESIAN_POINT ( 'NONE',  ( 47.68298272704948459, 153.7393326413893817, -9.013488496775837078 ) ) ;
#3627 = CARTESIAN_POINT ( 'NONE',  ( 40.27526882409969033, 90.56518717409400665, 37.97664729208901946 ) ) ;
#3629 = CARTESIAN_POINT ( 'NONE',  ( -161.4692556286852607, -194.3391397928654669, 52.90620854394536821 ) ) ;
#3630 = EDGE_CURVE ( 'NONE', #12363, #20108, #7922, .T. ) ;
#3631 = CARTESIAN_POINT ( 'NONE',  ( -154.3824083646099439, -176.4938272943107336, 40.69124936498395328 ) ) ;
#3632 = CARTESIAN_POINT ( 'NONE',  ( -149.8854112254399524, -178.6622583705452314, 59.65701158161632378 ) ) ;
#3633 = PLANE ( 'NONE',  #19511 ) ;
#3634 = CARTESIAN_POINT ( 'NONE',  ( 43.01140435219957681, 68.96049967264870872, 29.21067981925356705 ) ) ;
#3635 = PLANE ( 'NONE',  #18550 ) ;
#3636 = CARTESIAN_POINT ( 'NONE',  ( 46.59305225739526435, 151.5797705074273267, 36.81289934271958941 ) ) ;
#3637 = CARTESIAN_POINT ( 'NONE',  ( 44.37947211624943833, 107.4797705074273182, 30.00020018409699318 ) ) ;
#3638 = CARTESIAN_POINT ( 'NONE',  ( 34.41316853928974950, 153.0433231119815503, 10.55326060710041958 ) ) ;
#3639 = CARTESIAN_POINT ( 'NONE',  ( 38.58424406990786082, 132.1151871740940180, 34.21067981925357060 ) ) ;
#3640 = CARTESIAN_POINT ( 'NONE',  ( -151.4692556286852891, -178.4084106276440593, 59.56931450028537256 ) ) ;
#3641 = CARTESIAN_POINT ( 'NONE',  ( 45.74753988029934249, 62.06518717409399244, 30.44471234641812174 ) ) ;
#3642 = CARTESIAN_POINT ( 'NONE',  ( 69.03752116822961682, 130.9715778530742227, -2.776543650264200025 ) ) ;
#3643 = LINE ( 'NONE', #5186, #7066 ) ;
#3644 = CARTESIAN_POINT ( 'NONE',  ( 44.37947211624943833, 118.0151871740940095, 38.42115945441014446 ) ) ;
#3645 = ORIENTED_EDGE ( 'NONE', *, *, #15936, .F. ) ;
#3646 = EDGE_CURVE ( 'NONE', #12851, #32, #3464, .T. ) ;
#3647 = EDGE_LOOP ( 'NONE', ( #9210, #9558, #9741, #13451 ) ) ;
#3648 = FACE_OUTER_BOUND ( 'NONE', #12386, .T. ) ;
#3649 = VERTEX_POINT ( 'NONE', #14626 ) ;
#3650 = CARTESIAN_POINT ( 'NONE',  ( 38.01140435219951996, 101.6344580088725849, 32.58608133808903773 ) ) ;
#3651 = CARTESIAN_POINT ( 'NONE',  ( 40.27526882409969744, 156.8297705074272983, 37.97664729208901235 ) ) ;
#3652 = CARTESIAN_POINT ( 'NONE',  ( 39.92123440845004723, 157.1604996726487684, 38.46393386101376421 ) ) ;
#3654 = CARTESIAN_POINT ( 'NONE',  ( 25.00529828370466490, 141.4305569644042464, -16.86339438981633876 ) ) ;
#3653 = CARTESIAN_POINT ( 'NONE',  ( 46.59305225739526435, 112.9151871740940010, 31.60846029578754468 ) ) ;
#3655 = CARTESIAN_POINT ( 'NONE',  ( 39.92123440845004723, 75.26049967264873430, 29.95742577749337343 ) ) ;
#3657 = DIRECTION ( 'NONE',  ( 0.000000000000000000, 0.000000000000000000, 1.000000000000000000 ) ) ;
#3656 = DIRECTION ( 'NONE',  ( 0.000000000000000000, 0.000000000000000000, -1.000000000000000000 ) ) ;
#3658 = CARTESIAN_POINT ( 'NONE',  ( 41.64333658814960870, 74.51518717409399528, 30.00020018409699318 ) ) ;
#3659 = CARTESIAN_POINT ( 'NONE',  ( 134.6380592378700101, 268.5785371414991687, -19.99999999999997868 ) ) ;
#3660 = CARTESIAN_POINT ( 'NONE',  ( -160.8964159109769696, -184.8938272943107393, 49.65701158161630957 ) ) ;
#3661 = CARTESIAN_POINT ( 'NONE',  ( 138.5268905834513191, 193.0332408774651185, -50.99999999999998579 ) ) ;
#3662 = EDGE_CURVE ( 'NONE', #7305, #11189, #21769, .T. ) ;
#3663 = ORIENTED_EDGE ( 'NONE', *, *, #5564, .T. ) ;
#3664 = CARTESIAN_POINT ( 'NONE',  ( -159.0959885057557983, -187.8584106276440480, 55.19815736654470584 ) ) ;
#3665 = CARTESIAN_POINT ( 'NONE',  ( 75.40436159597490473, 130.9804297329818326, 12.22031048084446248 ) ) ;
#3666 = CARTESIAN_POINT ( 'NONE',  ( -154.3824083646099439, -176.7584106276440536, 40.69124936498395328 ) ) ;
#3667 = EDGE_LOOP ( 'NONE', ( #7526, #9262, #18046, #20185, #3337, #5414, #10888, #19284, #4437, #9397, #14577, #6175, #1280 ) ) ;
#3668 = CARTESIAN_POINT ( 'NONE',  ( 45.74753988029933538, 140.0651871740940067, 30.44471234641811819 ) ) ;
#3669 = CARTESIAN_POINT ( 'NONE',  ( -166.4803626276155626, -116.9891397928655010, 49.65701158161629536 ) ) ;
#3670 = CARTESIAN_POINT ( 'NONE',  ( 44.37947211624943833, 106.2797705074273154, 38.42115945441014446 ) ) ;
#3671 = CARTESIAN_POINT ( 'NONE',  ( 40.90832812944997698, 154.0758954209757121, 3.767805038447253452 ) ) ;
#3672 = ORIENTED_EDGE ( 'NONE', *, *, #238, .T. ) ;
#3673 = PRODUCT_RELATED_PRODUCT_CATEGORY ( 'part', '', ( #6562 ) ) ;
#3674 = ORIENTED_EDGE ( 'NONE', *, *, #13573, .T. ) ;
#3675 = VECTOR ( 'NONE', #19317, 1000.000000000000227 ) ;
#3676 = CARTESIAN_POINT ( 'NONE',  ( 43.01140435219951996, 10.71049967264875491, 39.21067981925356349 ) ) ;
#3677 = CARTESIAN_POINT ( 'NONE',  ( -151.4692556286852891, -136.9891397928655010, -64.65701158161634510 ) ) ;
#3678 = ADVANCED_FACE ( 'NONE', ( #18042, #6479, #16173 ), #7816, .F. ) ;
#3679 = CARTESIAN_POINT ( 'NONE',  ( 38.58424406990784661, 141.2651871740940237, 35.64915139335016647 ) ) ;
#3680 = EDGE_CURVE ( 'NONE', #17077, #17427, #12985, .T. ) ;
#3681 = CARTESIAN_POINT ( 'NONE',  ( 61.01612483116806374, 90.79174121657607088, -0.2798613066081144796 ) ) ;
#3682 = CARTESIAN_POINT ( 'NONE',  ( 44.55648932407425633, 119.8104996726487457, 29.45539723777780239 ) ) ;
#3683 = CARTESIAN_POINT ( 'NONE',  ( -151.4692556286852891, -174.2391397928655010, 39.14238933923362396 ) ) ;
#3684 = EDGE_CURVE ( 'NONE', #9201, #4525, #14843, .T. ) ;
#3685 = CARTESIAN_POINT ( 'NONE',  ( -159.5594255724347761, -181.2630981290893146, 55.53486410454104316 ) ) ;
#3686 = DIRECTION ( 'NONE',  ( 0.000000000000000000, 0.000000000000000000, 1.000000000000000000 ) ) ;
#3687 = FACE_OUTER_BOUND ( 'NONE', #19743, .T. ) ;
#3688 = CARTESIAN_POINT ( 'NONE',  ( 46.59305225739526435, 89.17977050742732104, 31.60846029578754468 ) ) ;
#3689 = CARTESIAN_POINT ( 'NONE',  ( 24.69269415895541542, 98.46806607146707790, -5.796035312751787849 ) ) ;
#3690 = CARTESIAN_POINT ( 'NONE',  ( -142.0420953463935803, -171.5438272943106881, 52.72008163687743831 ) ) ;
#3691 = AXIS2_PLACEMENT_3D ( 'NONE', #3167, #16597, #1514 ) ;
#3692 = CARTESIAN_POINT ( 'NONE',  ( 45.74753988029934249, 83.06518717409400665, 30.44471234641812174 ) ) ;
#3693 = FACE_OUTER_BOUND ( 'NONE', #13506, .T. ) ;
#3694 = CARTESIAN_POINT ( 'NONE',  ( -136.6255475934131596, 760.1741454933652449, -3.999999999999980904 ) ) ;
#3695 = EDGE_LOOP ( 'NONE', ( #5315, #463, #13343, #5988 ) ) ;
#3696 = CARTESIAN_POINT ( 'NONE',  ( -149.8854112254398956, -189.3160212151857422, 39.65701158161630246 ) ) ;
#3697 = DIRECTION ( 'NONE',  ( 0.000000000000000000, 0.000000000000000000, 1.000000000000000000 ) ) ;
#3698 = CARTESIAN_POINT ( 'NONE',  ( 22.73392375623628681, 139.3438357627746882, 11.01889030017397531 ) ) ;
#3699 = ORIENTED_EDGE ( 'NONE', *, *, #14722, .F. ) ;
#3700 = CARTESIAN_POINT ( 'NONE',  ( 39.42975644700377558, 60.07977050742731251, 31.60846029578754468 ) ) ;
#3701 = ORIENTED_EDGE ( 'NONE', *, *, #15830, .F. ) ;
#3702 = CARTESIAN_POINT ( 'NONE',  ( 38.58424406990784661, 135.2297705074273324, 32.77220824515698183 ) ) ;
#3703 = CARTESIAN_POINT ( 'NONE',  ( 39.42975644700377558, 93.67977050742732104, 36.81289934271958941 ) ) ;
#3704 = FACE_OUTER_BOUND ( 'NONE', #19461, .T. ) ;
#3705 = B_SPLINE_CURVE_WITH_KNOTS ( 'NONE', 3,
 ( #5406, #3764, #553, #10492, #15548, #17191, #2103, #8841, #7183, #12239, #2313, #3872, #17300, #14535, #14320, #19500, #1204, #17947, #7618, #2633, #21276, #19610, #6154, #9268, #21164, #12889, #990, #20949, #11124, #19393, #21062, #776, #4290, #2532, #4504, #1098, #9489, #11017 ),
 .UNSPECIFIED., .F., .F.,
 ( 4, 2, 2, 2, 2, 2, 2, 2, 2, 2, 2, 2, 2, 2, 2, 2, 2, 2, 4 ),
 ( 0.01567185795944686655, 0.01665109603395608165, 0.01763033410846529675, 0.01811995314571990950, 0.01860957218297452573, 0.01958881025748375124, 0.02056804833199297675, 0.02154728640650219532, 0.02252652448101141389, 0.02350576255552062899, 0.02448500063002984756, 0.02546423870453906613, 0.02644347677904828470, 0.02693309581630289051, 0.02742271485355749633, 0.02840195292806670796, 0.02938119100257591959, 0.03036042907708513122, 0.03133966715159434285 ),
 .UNSPECIFIED. ) ;
#3706 = CARTESIAN_POINT ( 'NONE',  ( 39.42975644700377558, 62.81518717409399954, 31.60846029578754468 ) ) ;
#3707 = DIRECTION ( 'NONE',  ( -0.000000000000000000, 1.000000000000000000, -0.000000000000000000 ) ) ;
#3708 = CARTESIAN_POINT ( 'NONE',  ( 39.42975644700377558, 101.8151871740940067, 31.60846029578754468 ) ) ;
#3709 = DIRECTION ( 'NONE',  ( 0.000000000000000000, 1.000000000000000000, 0.000000000000000000 ) ) ;
#3710 = CARTESIAN_POINT ( 'NONE',  ( 38.01140435219952707, 108.8604996726487144, 35.83527830041809636 ) ) ;
#3711 = CARTESIAN_POINT ( 'NONE',  ( -145.2889157411863721, -168.5130981290892578, 58.16351966513671812 ) ) ;
#3712 = CARTESIAN_POINT ( 'NONE',  ( 287.2758801270296658, 0.000000000000000000, -76.96938077665298295 ) ) ;
#3713 = AXIS2_PLACEMENT_3D ( 'NONE', #9112, #4032, #935 ) ;
#3714 = CARTESIAN_POINT ( 'NONE',  ( -153.0531000319306543, -190.8160212151857422, 59.65701158161630957 ) ) ;
#3715 = CARTESIAN_POINT ( 'NONE',  ( 38.01140435219951996, 137.9344580088726104, 35.83527830041810347 ) ) ;
#3716 = CARTESIAN_POINT ( 'NONE',  ( 43.01140435219951286, 124.1297705074272955, 38.86567161673127657 ) ) ;
#3717 = CARTESIAN_POINT ( 'NONE',  ( 17.08493018425929932, 131.2036312357472241, 1.628145005703640624 ) ) ;
#3718 = DIRECTION ( 'NONE',  ( -1.000000000000000000, 0.000000000000000000, 0.000000000000000000 ) ) ;
#3719 = CARTESIAN_POINT ( 'NONE',  ( 40.27526882409969744, 110.6651871740940010, 30.44471234641812174 ) ) ;
#3720 = CARTESIAN_POINT ( 'NONE',  ( 43.01140435219951996, 10.71049967264875491, 34.21067981925357060 ) ) ;
#3721 = CARTESIAN_POINT ( 'NONE',  ( 23.23160898551418185, 147.7622765488190453, -10.85157364460736140 ) ) ;
#3722 = EDGE_CURVE ( 'NONE', #5192, #5761, #11213, .T. ) ;
#3723 = CARTESIAN_POINT ( 'NONE',  ( 50.77370750611731154, 147.0167679772302165, 11.22784935402935957 ) ) ;
#3724 = CARTESIAN_POINT ( 'NONE',  ( -148.3790856849358306, -156.6630981290892919, 59.16757674456786020 ) ) ;
#3725 = CARTESIAN_POINT ( 'NONE',  ( 38.58424406990786082, 84.37977050742730967, 34.21067981925357060 ) ) ;
#3726 = ORIENTED_EDGE ( 'NONE', *, *, #349, .T. ) ;
#3727 = EDGE_CURVE ( 'NONE', #16987, #14880, #19708, .T. ) ;
#3728 = CARTESIAN_POINT ( 'NONE',  ( -143.9637021292201950, -116.9891397928655010, 62.65701158161630957 ) ) ;
#3729 = CARTESIAN_POINT ( 'NONE',  ( 38.96631938032478359, 71.48445800887257917, 31.27175355779120025 ) ) ;
#3730 = DIRECTION ( 'NONE',  ( 1.000000000000000000, 0.000000000000000000, -1.257660470541341077E-16 ) ) ;
#3731 = CARTESIAN_POINT ( 'NONE',  ( 38.01140435219951996, 126.5604996726487315, 32.58608133808903773 ) ) ;
#3733 = CARTESIAN_POINT ( 'NONE',  ( 13.64837572802379562, 102.4646860582014796, -11.51360178106338594 ) ) ;
#3732 = CARTESIAN_POINT ( 'NONE',  ( 40.27526882409969033, 87.56518717409400665, 37.97664729208901946 ) ) ;
#3734 =( BOUNDED_CURVE ( )  B_SPLINE_CURVE ( 2, ( #1358, #16444, #9747, #7874, #14573, #6428, #11379, #21209, #4766, #19538, #3121, #6091, #19767 ),
 .UNSPECIFIED., .F., .F. ) 
 B_SPLINE_CURVE_WITH_KNOTS ( ( 3, 2, 2, 2, 2, 2, 3 ),
 ( 0.8035714285714286031, 0.8071428571428571619, 0.8142857142857142794, 0.8214285714285713969, 0.8285714285714286254, 0.8357142857142857428, 0.8392857142857143016 ),
 .UNSPECIFIED. ) 
 CURVE ( )  GEOMETRIC_REPRESENTATION_ITEM ( )  RATIONAL_B_SPLINE_CURVE ( ( 0.9755282581475768211, 0.9755282581475768211, 1.000000000000000000, 0.9510565162951535312, 1.000000000000000000, 0.9510565162951535312, 1.000000000000000000, 0.9510565162951535312, 1.000000000000000000, 0.9510565162951535312, 1.000000000000000000, 0.9755282581475768211, 0.9755282581475768211 ) ) 
 REPRESENTATION_ITEM ( '' )  );
#3735 = CARTESIAN_POINT ( 'NONE',  ( -151.4692556286852891, -161.9084106276440593, 39.74470866294723947 ) ) ;
#3736 = CARTESIAN_POINT ( 'NONE',  ( -157.2955611005345986, -184.4438272943107506, 57.67623309621197336 ) ) ;
#3737 = LINE ( 'NONE', #2081, #14645 ) ;
#3738 = CARTESIAN_POINT ( 'NONE',  ( -154.5594255724347761, -194.1630981290892919, 40.14644641866476604 ) ) ;
#3739 = CARTESIAN_POINT ( 'NONE',  ( 43.01140435219951286, 92.03445800887257633, 29.21067981925356705 ) ) ;
#3740 = CARTESIAN_POINT ( 'NONE',  ( 0.000000000000000000, -116.9891397928655010, 0.000000000000000000 ) ) ;
#3741 = VECTOR ( 'NONE', #20560, 1000.000000000000000 ) ;
#3742 = CARTESIAN_POINT ( 'NONE',  ( 41.64333658814960870, 150.9797705074273324, 38.42115945441014446 ) ) ;
#3743 = CARTESIAN_POINT ( 'NONE',  ( 40.27526882409969033, 101.9297705074273068, 30.44471234641811819 ) ) ;
#3744 = CARTESIAN_POINT ( 'NONE',  ( 74.27779736592162863, 105.9683817680885056, 13.05343286460986363 ) ) ;
#3745 = CARTESIAN_POINT ( 'NONE',  ( 38.58424406990785371, 137.9651871740940123, 32.77220824515697473 ) ) ;
#3746 = CARTESIAN_POINT ( 'NONE',  ( -157.6495955161842062, -188.9391397928654328, 41.15050349809589392 ) ) ;
#3747 = CARTESIAN_POINT ( 'NONE',  ( -154.3824083646099439, -161.7584106276440252, 40.69124936498395328 ) ) ;
#3748 = VECTOR ( 'NONE', #18196, 1000.000000000000000 ) ;
#3749 = DIRECTION ( 'NONE',  ( -1.000000000000000000, 0.000000000000000000, 0.000000000000000000 ) ) ;
#3750 = CARTESIAN_POINT ( 'NONE',  ( 53.23527110998836775, 93.53878102080766155, -0.9907194398206048414 ) ) ;
#3751 = CARTESIAN_POINT ( 'NONE',  ( 84.42064422693164261, 282.0082918409407284, 272.0939500981630204 ) ) ;
#3752 = CARTESIAN_POINT ( 'NONE',  ( 44.37947211624943833, 112.0151871740940095, 38.42115945441014446 ) ) ;
#3753 = ORIENTED_EDGE ( 'NONE', *, *, #6972, .F. ) ;
#3754 = EDGE_CURVE ( 'NONE', #8983, #11479, #18131, .T. ) ;
#3755 = DIRECTION ( 'NONE',  ( 1.000000000000000000, 0.000000000000000000, -0.000000000000000000 ) ) ;
#3756 = ORIENTED_EDGE ( 'NONE', *, *, #1015, .T. ) ;
#3757 = CARTESIAN_POINT ( 'NONE',  ( 38.96631938032478359, 105.0844580088725877, 37.14960608071593384 ) ) ;
#3758 = AXIS2_PLACEMENT_3D ( 'NONE', #6028, #965, #2405 ) ;
#3759 = CARTESIAN_POINT ( 'NONE',  ( 38.58424406990786082, 150.3797705074273097, 34.21067981925357060 ) ) ;
#3760 = CARTESIAN_POINT ( 'NONE',  ( 46.10157429594899270, 154.7604996726487343, 38.46393386101376421 ) ) ;
#3762 = CARTESIAN_POINT ( 'NONE',  ( 35.06472793454997117, 92.93335285089702325, -12.26792952838020767 ) ) ;
#3761 = CARTESIAN_POINT ( 'NONE',  ( 38.58424406990784661, 113.9651871740940123, 32.77220824515698183 ) ) ;
#3763 = CARTESIAN_POINT ( 'NONE',  ( 38.01140435219952707, 69.71049967264873715, 34.21067981925357060 ) ) ;
#3765 = CARTESIAN_POINT ( 'NONE',  ( 91.17254549292282206, -61.68114226949890622, 20.00000000000000355 ) ) ;
#3764 = CARTESIAN_POINT ( 'NONE',  ( 43.33809753620296590, 144.9070776186055696, 29.21067981925357060 ) ) ;
#3766 = CARTESIAN_POINT ( 'NONE',  ( 138.4260920561042667, 141.9264758756783351, -5.999999999999976019 ) ) ;
#3767 = CARTESIAN_POINT ( 'NONE',  ( 46.77903254544086309, 95.19149378333804634, 30.90720150815159784 ) ) ;
#3768 = CARTESIAN_POINT ( 'NONE',  ( 44.37947211624943833, 83.21518717409399812, 30.00020018409699318 ) ) ;
#3769 = CARTESIAN_POINT ( 'NONE',  ( 41.46631938032478359, 64.31049967264873146, 38.96596240072933170 ) ) ;
#3770 = CARTESIAN_POINT ( 'NONE',  ( -142.0420953463935803, -177.2438272943107620, 46.59394152635518793 ) ) ;
#3771 = CARTESIAN_POINT ( 'NONE',  ( -160.8964159109769696, -194.3084106276440366, 46.59394152635518083 ) ) ;
#3772 = ORIENTED_EDGE ( 'NONE', *, *, #2599, .T. ) ;
#3773 = CARTESIAN_POINT ( 'NONE',  ( -151.4692556286852891, -178.4084106276440878, 59.56931450028537967 ) ) ;
#3774 = VECTOR ( 'NONE', #8378, 1000.000000000000000 ) ;
#3775 = CARTESIAN_POINT ( 'NONE',  ( 9.976645104453018220, 110.9295780357170571, 15.79146183154218619 ) ) ;
#3776 = EDGE_LOOP ( 'NONE', ( #15667, #19204 ) ) ;
#3777 = CARTESIAN_POINT ( 'NONE',  ( 39.42975644700377558, 147.4151871740940294, 36.81289934271958941 ) ) ;
#3778 = CARTESIAN_POINT ( 'NONE',  ( -55.11860757350579831, 784.8075632535900468, -3.999999999999996447 ) ) ;
#3779 = CARTESIAN_POINT ( 'NONE',  ( 45.74753988029934249, 106.4297705074273210, 37.97664729208901235 ) ) ;
#3780 = CARTESIAN_POINT ( 'NONE',  ( 58.57487293839693621, 150.3975950434478648, 4.362879525569486994 ) ) ;
#3781 = EDGE_LOOP ( 'NONE', ( #21421, #9964, #17959, #6535 ) ) ;
#3782 = CARTESIAN_POINT ( 'NONE',  ( 28.62772086389876947, 95.65184626908498444, 8.013395860235284829 ) ) ;
#3783 = ORIENTED_EDGE ( 'NONE', *, *, #14965, .F. ) ;
#3784 = CARTESIAN_POINT ( 'NONE',  ( 43.01140435219951286, 113.6297705074273097, 29.55568802177586463 ) ) ;
#3785 = AXIS2_PLACEMENT_3D ( 'NONE', #1057, #19682, #21452 ) ;
#3786 = CARTESIAN_POINT ( 'NONE',  ( 126.8576204525573274, -126.9891397928655010, -17.64809332337413750 ) ) ;
#3787 = CARTESIAN_POINT ( 'NONE',  ( 41.46631938032478359, 126.1104996726487570, 29.45539723777780239 ) ) ;
#3788 = CARTESIAN_POINT ( 'NONE',  ( 39.42975644700377558, 147.4151871740940294, 36.81289934271958941 ) ) ;
#3789 = AXIS2_PLACEMENT_3D ( 'NONE', #3084, #18514, #10036 ) ;
#3790 = CARTESIAN_POINT ( 'NONE',  ( 38.01140435219951996, 99.86049967264871441, 35.83527830041810347 ) ) ;
#3791 = CARTESIAN_POINT ( 'NONE',  ( 64.11693453485118255, 146.8606268255622638, -2.422805558527139080 ) ) ;
#3792 = CARTESIAN_POINT ( 'NONE',  ( 41.46631938032478359, 61.31049967264873146, 38.96596240072933170 ) ) ;
#3793 = CARTESIAN_POINT ( 'NONE',  ( -161.4692556286853176, -170.4891397928654726, 49.65701158161630957 ) ) ;
#3794 = CARTESIAN_POINT ( 'NONE',  ( -157.6495955161842062, -182.0130981290893146, 41.15050349809589392 ) ) ;
#3795 = CYLINDRICAL_SURFACE ( 'NONE', #8313, 10.00000000000000888 ) ;
#3796 = CARTESIAN_POINT ( 'NONE',  ( 156.1725454929228079, -61.68114226949890622, 30.00000000000000000 ) ) ;
#3797 = EDGE_CURVE ( 'NONE', #18561, #13046, #19819, .T. ) ;
#3798 = CARTESIAN_POINT ( 'NONE',  ( 45.74753988029933538, 89.32977050742732672, 30.44471234641811819 ) ) ;
#3799 = CARTESIAN_POINT ( 'NONE',  ( -159.0959885057557983, -175.5938272943107279, 55.19815736654470584 ) ) ;
#3800 = CARTESIAN_POINT ( 'NONE',  ( 41.64333658814960870, 78.71518717409399812, 38.42115945441014446 ) ) ;
#3802 = CIRCLE ( 'NONE', #18591, 10.00000000000000888 ) ;
#3801 = DIRECTION ( 'NONE',  ( -0.9385982292947087080, -0.3450121214752279175, 0.000000000000000000 ) ) ;
#3803 = FACE_OUTER_BOUND ( 'NONE', #16547, .T. ) ;
#3804 = ORIENTED_EDGE ( 'NONE', *, *, #1285, .F. ) ;
#3805 = VECTOR ( 'NONE', #20027, 1000.000000000000000 ) ;
#3806 = DIRECTION ( 'NONE',  ( 0.9385982292947087080, 0.3450121214752278620, 0.000000000000000000 ) ) ;
#3807 = CARTESIAN_POINT ( 'NONE',  ( 47.43856463449117911, 130.7297705074273040, 35.64915139335015937 ) ) ;
#3808 = CARTESIAN_POINT ( 'NONE',  ( 56.57648482392179545, 95.27494636639178793, 7.851242587554376762 ) ) ;
#3809 = VERTEX_POINT ( 'NONE', #21588 ) ;
#3810 = AXIS2_PLACEMENT_3D ( 'NONE', #10387, #6975, #17304 ) ;
#3811 = CARTESIAN_POINT ( 'NONE',  ( 44.55648932407425633, 73.88445800887258486, 29.45539723777780239 ) ) ;
#3812 = ORIENTED_EDGE ( 'NONE', *, *, #238, .F. ) ;
#3813 = CARTESIAN_POINT ( 'NONE',  ( 39.42975644700377558, 132.6797705074273210, 36.81289934271958941 ) ) ;
#3814 = CARTESIAN_POINT ( 'NONE',  ( -143.3790856849358306, -181.2891397928654840, 55.53486410454105027 ) ) ;
#3815 = CARTESIAN_POINT ( 'NONE',  ( -141.4692556286852891, -195.9891397928654726, 49.65701158161630957 ) ) ;
#3816 = CARTESIAN_POINT ( 'NONE',  ( 41.64333658814960870, 98.51518717409399528, 30.00020018409699318 ) ) ;
#3817 = CARTESIAN_POINT ( 'NONE',  ( -148.5561028927606344, -156.9938272943107052, 58.62277379824867296 ) ) ;
#3818 = CARTESIAN_POINT ( 'NONE',  ( 41.46631938032478359, 108.1104996726487428, 29.45539723777780239 ) ) ;
#3819 = CARTESIAN_POINT ( 'NONE',  ( -157.6495955161842062, -169.1130981290893374, 58.16351966513671812 ) ) ;
#3821 = VECTOR ( 'NONE', #14431, 1000.000000000000000 ) ;
#3820 = CARTESIAN_POINT ( 'NONE',  ( 0.000000000000000000, 0.000000000000000000, 0.000000000000000000 ) ) ;
#3822 = CARTESIAN_POINT ( 'NONE',  ( 131.8222645499855901, 267.5435007770738025, -6.999999999999995559 ) ) ;
#3823 = CARTESIAN_POINT ( 'NONE',  ( 38.01140435219951996, 143.6344580088725422, 32.58608133808903773 ) ) ;
#3824 = CARTESIAN_POINT ( 'NONE',  ( 41.64333658814960870, 108.9797705074273324, 38.42115945441014446 ) ) ;
#3825 = CARTESIAN_POINT ( 'NONE',  ( 27.23529593042425390, 96.43589704216468306, 0.08059930645588880838 ) ) ;
#3826 = CARTESIAN_POINT ( 'NONE',  ( 43.01140435219950575, 140.0344580088726332, 29.21067981925357060 ) ) ;
#3827 = CARTESIAN_POINT ( 'NONE',  ( 43.01140435219951286, 110.3651871740939896, 29.55568802177586107 ) ) ;
#3828 = VERTEX_POINT ( 'NONE', #19934 ) ;
#3829 = CARTESIAN_POINT ( 'NONE',  ( 42.21948215057684450, 88.38361825032848174, 39.21067981925355639 ) ) ;
#3830 = CARTESIAN_POINT ( 'NONE',  ( 10.42839491720816625, 130.4056617841633283, -4.565575592310756825 ) ) ;
#3831 = CARTESIAN_POINT ( 'NONE',  ( 33.52710748945926866, 93.34978808121778115, 14.79936193957723312 ) ) ;
#3832 = CARTESIAN_POINT ( 'NONE',  ( -141.4692556286852891, -168.9891397928654726, 49.65701158161630957 ) ) ;
#3833 = ADVANCED_FACE ( 'NONE', ( #16828 ), #15183, .F. ) ;
#3834 = CARTESIAN_POINT ( 'NONE',  ( 39.42975644700377558, 87.67977050742732104, 36.81289934271958941 ) ) ;
#3835 = EDGE_CURVE ( 'NONE', #11879, #1138, #3617, .T. ) ;
#3836 = ORIENTED_EDGE ( 'NONE', *, *, #268, .T. ) ;
#3837 = CARTESIAN_POINT ( 'NONE',  ( 46.10157429594899270, 75.83445800887258770, 38.46393386101376421 ) ) ;
#3838 = LINE ( 'NONE', #17160, #20393 ) ;
#3839 = CARTESIAN_POINT ( 'NONE',  ( 43.01140435219951286, 127.4604996726487514, 39.46799094044489209 ) ) ;
#3841 = CARTESIAN_POINT ( 'NONE',  ( 77.13564277734779751, 118.5067815986552375, -14.37074460762677397 ) ) ;
#3840 = CARTESIAN_POINT ( 'NONE',  ( 38.58424406990784661, 89.96518717409399812, 32.77220824515698183 ) ) ;
#3842 = CARTESIAN_POINT ( 'NONE',  ( -159.0959885057557983, -157.8584106276440480, 55.19815736654470584 ) ) ;
#3843 = CARTESIAN_POINT ( 'NONE',  ( -142.0420953463935803, -183.5438272943107449, 52.72008163687743831 ) ) ;
#3844 = DIRECTION ( 'NONE',  ( 0.000000000000000000, 1.000000000000000000, 0.000000000000000000 ) ) ;
#3845 = CARTESIAN_POINT ( 'NONE',  ( 44.55648932407425633, 127.8844580088725706, 29.45539723777780239 ) ) ;
#3846 = CARTESIAN_POINT ( 'NONE',  ( 38.01140435219952707, 80.93445800887256780, 35.83527830041809636 ) ) ;
#3847 = CARTESIAN_POINT ( 'NONE',  ( 43.01140435219951996, 10.71049967264875491, 34.21067981925357060 ) ) ;
#3848 = CARTESIAN_POINT ( 'NONE',  ( -151.4692556286852891, -195.9891397928654726, 59.65701158161632378 ) ) ;
#3849 = CARTESIAN_POINT ( 'NONE',  ( 45.74753988029933538, 139.4297705074272926, 37.97664729208901946 ) ) ;
#3850 = CARTESIAN_POINT ( 'NONE',  ( 46.59305225739526435, 101.1797705074273210, 31.60846029578754468 ) ) ;
#3851 = CARTESIAN_POINT ( 'NONE',  ( 30.18028515090226449, 151.2280014487717779, 17.43780275515692679 ) ) ;
#3852 = CARTESIAN_POINT ( 'NONE',  ( 40.27526882409969744, 138.5651871740939782, 37.97664729208901235 ) ) ;
#3853 = CARTESIAN_POINT ( 'NONE',  ( 44.55648932407425633, 67.88445800887258486, 29.45539723777780239 ) ) ;
#3854 = CARTESIAN_POINT ( 'NONE',  ( -159.0959885057557983, -163.8584106276440480, 55.19815736654470584 ) ) ;
#3855 = EDGE_CURVE ( 'NONE', #8015, #10293, #8796, .T. ) ;
#3856 = AXIS2_PLACEMENT_3D ( 'NONE', #9588, #21159, #4387 ) ;
#3857 = CARTESIAN_POINT ( 'NONE',  ( 39.42975644700377558, 63.67977050742732104, 36.81289934271958941 ) ) ;
#3858 = CARTESIAN_POINT ( 'NONE',  ( 68.27453032555700929, 132.6178071945132046, 11.15186410612756696 ) ) ;
#3859 = DIRECTION ( 'NONE',  ( 0.000000000000000000, 1.000000000000000000, 0.000000000000000000 ) ) ;
#3860 = CARTESIAN_POINT ( 'NONE',  ( 44.37947211624943833, 113.2151871740940123, 30.00020018409699318 ) ) ;
#3861 = ORIENTED_EDGE ( 'NONE', *, *, #15351, .F. ) ;
#3862 = CARTESIAN_POINT ( 'NONE',  ( 43.01140435219951286, 134.0344580088725763, 29.21067981925356705 ) ) ;
#3863 = VERTEX_POINT ( 'NONE', #5369 ) ;
#3864 =( BOUNDED_CURVE ( )  B_SPLINE_CURVE ( 2, ( #11890, #3523, #17272, #7158, #7267, #11994, #13968, #8593, #20707, #12315, #1863, #5484, #13861 ),
 .UNSPECIFIED., .F., .F. ) 
 B_SPLINE_CURVE_WITH_KNOTS ( ( 3, 2, 2, 2, 2, 2, 3 ),
 ( 0.4044117647058823595, 0.4058823529411764719, 0.4088235294117646967, 0.4117647058823529216, 0.4147058823529412019, 0.4176470588235294268, 0.4191176470588235392 ),
 .UNSPECIFIED. ) 
 CURVE ( )  GEOMETRIC_REPRESENTATION_ITEM ( )  RATIONAL_B_SPLINE_CURVE ( ( 0.9755282581475768211, 0.9755282581475768211, 1.000000000000000000, 0.9510565162951535312, 1.000000000000000000, 0.9510565162951535312, 1.000000000000000000, 0.9510565162951535312, 1.000000000000000000, 0.9510565162951535312, 1.000000000000000000, 0.9755282581475768211, 0.9755282581475768211 ) ) 
 REPRESENTATION_ITEM ( '' )  );
#3865 = CARTESIAN_POINT ( 'NONE',  ( 47.05648932407426344, 105.9844580088725792, 37.14960608071593384 ) ) ;
#3866 = CARTESIAN_POINT ( 'NONE',  ( 38.58424406990785371, 147.5297705074273154, 35.64915139335015937 ) ) ;
#3867 =( GEOMETRIC_REPRESENTATION_CONTEXT ( 3 ) GLOBAL_UNCERTAINTY_ASSIGNED_CONTEXT ( ( #1816 ) ) GLOBAL_UNIT_ASSIGNED_CONTEXT ( ( #4027, #8894, #9109 ) ) REPRESENTATION_CONTEXT ( 'NONE', 'WORKASPACE' ) );
#3868 = CARTESIAN_POINT ( 'NONE',  ( 39.92123440845004723, 159.2604996726487343, 29.95742577749337343 ) ) ;
#3870 = CARTESIAN_POINT ( 'NONE',  ( 19.52755003174225124, 104.2962547294809070, 15.51356631106660089 ) ) ;
#3869 = CARTESIAN_POINT ( 'NONE',  ( 41.64333658814960870, 120.7151871740939981, 38.42115945441014446 ) ) ;
#3871 = CARTESIAN_POINT ( 'NONE',  ( 46.10157429594899270, 68.66049967264873999, 29.95742577749337343 ) ) ;
#3873 = DIRECTION ( 'NONE',  ( -0.000000000000000000, -0.000000000000000000, -1.000000000000000000 ) ) ;
#3872 = CARTESIAN_POINT ( 'NONE',  ( 46.77550672146314525, 144.6231811833137044, 30.90345582088290044 ) ) ;
#3874 = CARTESIAN_POINT ( 'NONE',  ( 156.1725454929228079, -61.68114226949890622, 20.00000000000001776 ) ) ;
#3875 = CARTESIAN_POINT ( 'NONE',  ( 47.85069476305888259, 95.37983616430958023, 35.51056251760059013 ) ) ;
#3876 = CARTESIAN_POINT ( 'NONE',  ( 47.43856463449117200, 79.76518717409400949, 32.77220824515698183 ) ) ;
#3877 = LINE ( 'NONE', #5737, #1322 ) ;
#3878 = CARTESIAN_POINT ( 'NONE',  ( -151.4692556286852891, -185.6438272943107393, 39.74470866294723947 ) ) ;
#3879 = CARTESIAN_POINT ( 'NONE',  ( -154.3824083646099439, -194.7584106276440536, 40.69124936498395328 ) ) ;
#3880 = ORIENTED_EDGE ( 'NONE', *, *, #3046, .F. ) ;
#3881 = CARTESIAN_POINT ( 'NONE',  ( -160.8964159109769696, -179.1584106276440309, 49.65701158161630957 ) ) ;
#3882 = CARTESIAN_POINT ( 'NONE',  ( 76.06694498870253085, 129.1134374410657983, 4.287174360044270216 ) ) ;
#3883 = ORIENTED_EDGE ( 'NONE', *, *, #18144, .F. ) ;
#3884 = CARTESIAN_POINT ( 'NONE',  ( 40.27526882409969033, 143.6651871740940294, 30.44471234641811819 ) ) ;
#3885 = AXIS2_PLACEMENT_3D ( 'NONE', #14223, #20963, #12578 ) ;
#3886 = PRODUCT_DEFINITION_FORMATION_WITH_SPECIFIED_SOURCE ( 'ANY', '', #9956, .NOT_KNOWN. ) ;
#3887 = DIRECTION ( 'NONE',  ( 0.000000000000000000, 0.000000000000000000, 1.000000000000000000 ) ) ;
#3888 = CARTESIAN_POINT ( 'NONE',  ( 44.37947211624943833, 104.4797705074273182, 30.00020018409699318 ) ) ;
#3889 = CARTESIAN_POINT ( 'NONE',  ( 72.98789752971651978, 103.3738663174133023, 6.148623012889737005 ) ) ;
#3890 = EDGE_LOOP ( 'NONE', ( #1251, #13688, #12799, #9181 ) ) ;
#3891 = CARTESIAN_POINT ( 'NONE',  ( 70.94289844336020678, 123.7826807253454575, 5.513563639855703080 ) ) ;
#3892 = EDGE_LOOP ( 'NONE', ( #2122, #20671, #20776, #16006 ) ) ;
#3893 = CARTESIAN_POINT ( 'NONE',  ( 44.37947211624943833, 112.2797705074273296, 38.42115945441014446 ) ) ;
#3894 = DIRECTION ( 'NONE',  ( 0.000000000000000000, 0.000000000000000000, 1.000000000000000000 ) ) ;
#3895 = FACE_OUTER_BOUND ( 'NONE', #4743, .T. ) ;
#3896 = CARTESIAN_POINT ( 'NONE',  ( 47.43856463449117200, 148.7651871740939953, 32.77220824515698183 ) ) ;
#3897 = CARTESIAN_POINT ( 'NONE',  ( 39.92123440845004723, 97.16049967264873999, 38.46393386101376421 ) ) ;
#3898 = CARTESIAN_POINT ( 'NONE',  ( 64.59149290518072917, 93.33317027722591774, -7.422718449586769296 ) ) ;
#3899 = CLOSED_SHELL ( 'NONE', ( #15299, #15258, #14468, #17155, #3968, #19683, #5754, #19253, #19207, #16445, #5478, #12494, #18413, #8421, #471, #2577, #5734, #4224, #95, #1141, #12963, #8690, #8430, #3122, #7394, #16637, #3070, #2870, #4361, #7557, #12193, #8612, #3415, #19344, #4485, #6002, #18639, #10349, #14764, #15015, #16830, #489, #56, #9207, #16582, #8314, #16210, #4604, #15999, #2704, #4338, #18903, #18604, #6410, #7198, #13751, #6826, #13691, #21758, #4024, #17971, #19659, #997, #20371, #15546, #8580, #3045, #12810, #446, #7597, #397, #16526, #19946, #14340, #5854, #11460, #3405, #10106 ) ) ;
#3900 = CARTESIAN_POINT ( 'NONE',  ( -56.84366818088135176, 789.5005544000622422, -19.99999999999997868 ) ) ;
#3901 = CARTESIAN_POINT ( 'NONE',  ( -154.5594255724347761, -168.0891397928654669, 40.14644641866476604 ) ) ;
#3902 = CARTESIAN_POINT ( 'NONE',  ( 42.21948215057684450, 152.1113394311928175, 29.21067981925356705 ) ) ;
#3903 = ADVANCED_FACE ( 'NONE', ( #13739 ), #8684, .T. ) ;
#3904 = DIRECTION ( 'NONE',  ( -0.000000000000000000, 1.000000000000000000, -0.000000000000000000 ) ) ;
#3905 = CARTESIAN_POINT ( 'NONE',  ( -141.4692556286852891, -196.9891397928655010, 49.65701158161630957 ) ) ;
#3906 = ORIENTED_EDGE ( 'NONE', *, *, #980, .F. ) ;
#3907 = CARTESIAN_POINT ( 'NONE',  ( 40.27526882409969033, 83.92977050742732104, 30.44471234641811819 ) ) ;
#3908 = CARTESIAN_POINT ( 'NONE',  ( -159.0959885057557983, -163.5938272943107279, 55.19815736654470584 ) ) ;
#3909 = CARTESIAN_POINT ( 'NONE',  ( 38.58424406990786082, 81.11518717409398960, 34.21067981925357060 ) ) ;
#3910 = DIRECTION ( 'NONE',  ( 0.000000000000000000, 0.000000000000000000, 1.000000000000000000 ) ) ;
#3911 = ORIENTED_EDGE ( 'NONE', *, *, #1747, .F. ) ;
#3912 = LINE ( 'NONE', #4228, #8366 ) ;
#3913 = CARTESIAN_POINT ( 'NONE',  ( -133.8097529055291943, 761.2091818577913500, -45.62971374797768220 ) ) ;
#3914 = CARTESIAN_POINT ( 'NONE',  ( 45.74753988029934249, 134.3297705074273267, 30.44471234641812174 ) ) ;
#3915 = CARTESIAN_POINT ( 'NONE',  ( 15.29689364450883815, 124.6620785063593786, 10.35143954082134954 ) ) ;
#3916 = ORIENTED_EDGE ( 'NONE', *, *, #17917, .F. ) ;
#3917 = DIRECTION ( 'NONE',  ( 0.000000000000000000, 0.000000000000000000, -1.000000000000000000 ) ) ;
#3918 = ORIENTED_EDGE ( 'NONE', *, *, #14401, .T. ) ;
#3919 = CARTESIAN_POINT ( 'NONE',  ( 40.27526882409969033, 134.9297705074272926, 30.44471234641811819 ) ) ;
#3920 = CARTESIAN_POINT ( 'NONE',  ( 18.67254549292281141, -61.68114226949890622, -46.21320343559645494 ) ) ;
#3921 = CARTESIAN_POINT ( 'NONE',  ( 163.3215298332769407, 191.7840731147956319, 22.69574685642843193 ) ) ;
#3922 =( BOUNDED_CURVE ( )  B_SPLINE_CURVE ( 2, ( #2481, #21419, #10762, #6308, #13035, #728, #4654, #9003, #17467, #2378, #15714, #12517, #15814 ),
 .UNSPECIFIED., .F., .F. ) 
 B_SPLINE_CURVE_WITH_KNOTS ( ( 3, 2, 2, 2, 2, 2, 3 ),
 ( 0.8602941176470588758, 0.8617647058823529882, 0.8647058823529412130, 0.8676470588235294379, 0.8705882352941176627, 0.8735294117647058876, 0.8750000000000000000 ),
 .UNSPECIFIED. ) 
 CURVE ( )  GEOMETRIC_REPRESENTATION_ITEM ( )  RATIONAL_B_SPLINE_CURVE ( ( 0.9755282581475768211, 0.9755282581475777093, 1.000000000000000000, 0.9510565162951535312, 1.000000000000000000, 0.9510565162951535312, 1.000000000000000000, 0.9510565162951535312, 1.000000000000000000, 0.9510565162951535312, 1.000000000000000000, 0.9755282581475768211, 0.9755282581475768211 ) ) 
 REPRESENTATION_ITEM ( '' )  );
#3923 = CARTESIAN_POINT ( 'NONE',  ( 44.37947211624943833, 95.21518717409399812, 30.00020018409699318 ) ) ;
#3924 = CARTESIAN_POINT ( 'NONE',  ( 151.4773229304660731, 84.89323405393692212, -19.99999999999997868 ) ) ;
#3925 = CARTESIAN_POINT ( 'NONE',  ( 162.3411339277076308, 184.7625696037766261, -19.99999999999997868 ) ) ;
#3926 = CARTESIAN_POINT ( 'NONE',  ( -154.5594255724347761, -159.9630981290893317, 59.16757674456785310 ) ) ;
#3927 = DIRECTION ( 'NONE',  ( 0.000000000000000000, 0.000000000000000000, 1.000000000000000000 ) ) ;
#3928 = CARTESIAN_POINT ( 'NONE',  ( 43.01140435219951286, 137.0344580088725479, 28.95336869806222779 ) ) ;
#3929 = CARTESIAN_POINT ( 'NONE',  ( 43.01140435219951286, 116.6297705074273097, 29.55568802177586463 ) ) ;
#3930 = CARTESIAN_POINT ( 'NONE',  ( 22.02512380705847406, 92.75866610308527527, 21.07306443996510481 ) ) ;
#3931 = CARTESIAN_POINT ( 'NONE',  ( -142.0420953463936087, -195.3938272943107393, 49.65701158161630957 ) ) ;
#3932 = CARTESIAN_POINT ( 'NONE',  ( 47.43856463449117911, 106.7651871740939811, 32.77220824515697473 ) ) ;
#3933 = ORIENTED_EDGE ( 'NONE', *, *, #13644, .T. ) ;
#3934 = DIRECTION ( 'NONE',  ( -0.000000000000000000, -0.000000000000000000, -1.000000000000000000 ) ) ;
#3935 = EDGE_CURVE ( 'NONE', #14777, #14246, #412, .T. ) ;
#3936 = CARTESIAN_POINT ( 'NONE',  ( 28.88048086162541850, 151.0887240815949895, -10.63664014359656385 ) ) ;
#3937 = CARTESIAN_POINT ( 'NONE',  ( 19.23080508249268661, 135.0620028898917440, 9.799277925644819476 ) ) ;
#3938 = CARTESIAN_POINT ( 'NONE',  ( -149.8854112254399240, -168.3160212151857138, 39.65701158161629536 ) ) ;
#3939 = AXIS2_PLACEMENT_3D ( 'NONE', #14788, #9739, #2006 ) ;
#3940 = VECTOR ( 'NONE', #21428, 1000.000000000000227 ) ;
#3941 = CARTESIAN_POINT ( 'NONE',  ( 41.64333658814960870, 74.77977050742731535, 30.00020018409699318 ) ) ;
#3942 = ORIENTED_EDGE ( 'NONE', *, *, #8167, .F. ) ;
#3943 = CONICAL_SURFACE ( 'NONE', #21189, 9.000000000000007105, 0.7853981633974346233 ) ;
#3944 = CARTESIAN_POINT ( 'NONE',  ( 44.55648932407425633, 63.68445800887258201, 38.96596240072933170 ) ) ;
#3945 = CARTESIAN_POINT ( 'NONE',  ( -151.4692556286852607, -172.7391397928654726, 59.65701158161632378 ) ) ;
#3947 = EDGE_CURVE ( 'NONE', #16997, #8015, #3802, .T. ) ;
#3946 = CARTESIAN_POINT ( 'NONE',  ( 43.01140435219951286, 125.9604996726487514, 28.95336869806222779 ) ) ;
#3949 = CARTESIAN_POINT ( 'NONE',  ( 8.933461960486459574, 117.6319094064757422, 3.010161695468211551 ) ) ;
#3948 = CARTESIAN_POINT ( 'NONE',  ( 47.43856463449117200, 76.76518717409398107, 32.77220824515698183 ) ) ;
#3950 = CARTESIAN_POINT ( 'NONE',  ( -143.8425227516148084, -183.6938272943107506, 55.19815736654470584 ) ) ;
#3951 = CARTESIAN_POINT ( 'NONE',  ( 18.14018356548558941, 143.3940520581896862, 16.92415443696469879 ) ) ;
#3952 = CARTESIAN_POINT ( 'NONE',  ( -145.2889157411863721, -188.6130981290893089, 41.15050349809590102 ) ) ;
#3953 =( NAMED_UNIT ( * ) PLANE_ANGLE_UNIT ( ) SI_UNIT ( $, .RADIAN. ) );
#3954 = CIRCLE ( 'NONE', #12396, 5.000000000000004441 ) ;
#3955 = VECTOR ( 'NONE', #6141, 1000.000000000000000 ) ;
#3956 = DIRECTION ( 'NONE',  ( 0.000000000000000000, 0.000000000000000000, 1.000000000000000000 ) ) ;
#3957 = CARTESIAN_POINT ( 'NONE',  ( -134.9004869860375777, 755.4811543468929358, -19.99999999999996092 ) ) ;
#3958 = CARTESIAN_POINT ( 'NONE',  ( 41.64333658814960870, 137.7797705074273154, 30.00020018409699318 ) ) ;
#3959 = CARTESIAN_POINT ( 'NONE',  ( 39.42975644700377558, 105.6797705074273352, 36.81289934271958941 ) ) ;
#3960 = ADVANCED_FACE ( 'NONE', ( #13848 ), #20583, .T. ) ;
#3961 = CARTESIAN_POINT ( 'NONE',  ( 24.41145734808947054, 148.6458414325078081, 10.19629000755267434 ) ) ;
#3962 = CARTESIAN_POINT ( 'NONE',  ( 39.42975644700377558, 137.8151871740940067, 31.60846029578754468 ) ) ;
#3963 = CARTESIAN_POINT ( 'NONE',  ( 44.55648932407425633, 66.68445800887256780, 38.96596240072933170 ) ) ;
#3964 = CARTESIAN_POINT ( 'NONE',  ( -160.8964159109769696, -161.1584106276440593, 49.65701158161630957 ) ) ;
#3965 = CARTESIAN_POINT ( 'NONE',  ( -159.5594255724347761, -164.7891397928654555, 43.77915905869157598 ) ) ;
#3966 = CARTESIAN_POINT ( 'NONE',  ( 38.96631938032478359, 136.0104996726487627, 37.14960608071593384 ) ) ;
#3967 = CARTESIAN_POINT ( 'NONE',  ( 22.35924357203464297, 139.2281224154095014, 9.009280560090923373 ) ) ;
#3968 = ADVANCED_FACE ( 'NONE', ( #10013 ), #10449, .T. ) ;
#3969 = CARTESIAN_POINT ( 'NONE',  ( 41.64333658814960870, 110.5151871740940095, 30.00020018409699318 ) ) ;
#3970 = SHAPE_REPRESENTATION ( 'Hinges', ( #12657 ), #1776 ) ;
#3971 = ORIENTED_EDGE ( 'NONE', *, *, #5276, .T. ) ;
#3972 = CARTESIAN_POINT ( 'NONE',  ( -154.5594255724347761, -159.9630981290893317, 59.16757674456785310 ) ) ;
#3973 = ORIENTED_EDGE ( 'NONE', *, *, #14257, .F. ) ;
#3974 = CARTESIAN_POINT ( 'NONE',  ( 44.55648932407425633, 94.88445800887257064, 29.45539723777780239 ) ) ;
#3975 = CARTESIAN_POINT ( 'NONE',  ( 38.01140435219951996, 156.5604996726487457, 32.58608133808903773 ) ) ;
#3977 = CARTESIAN_POINT ( 'NONE',  ( 62.76710561173204894, 139.9178416638646638, -8.219927273936241008 ) ) ;
#3976 = CARTESIAN_POINT ( 'NONE',  ( 39.42975644700377558, 113.8151871740940067, 31.60846029578754468 ) ) ;
#3978 = CARTESIAN_POINT ( 'NONE',  ( 44.55648932407425633, 70.61049967264872862, 38.96596240072933170 ) ) ;
#3980 = DIRECTION ( 'NONE',  ( 0.000000000000000000, 1.000000000000000000, 0.000000000000000000 ) ) ;
#3979 = DIRECTION ( 'NONE',  ( 1.000000000000000000, 0.000000000000000000, 0.000000000000000000 ) ) ;
#3981 = CARTESIAN_POINT ( 'NONE',  ( 43.01140435219951286, 81.53445800887257633, 39.21067981925356349 ) ) ;
#3982 = EDGE_CURVE ( 'NONE', #21451, #14880, #13576, .T. ) ;
#3983 = DIRECTION ( 'NONE',  ( 0.000000000000000000, 0.000000000000000000, 1.000000000000000000 ) ) ;
#3984 = CARTESIAN_POINT ( 'NONE',  ( 47.49650721231805761, 95.31256562107512309, 31.99467674420385777 ) ) ;
#3985 = CARTESIAN_POINT ( 'NONE',  ( 45.74753988029933538, 71.06518717409400665, 30.44471234641811819 ) ) ;
#3986 = DIRECTION ( 'NONE',  ( 1.723963091245776585E-16, 6.336983651701954299E-17, 1.000000000000000000 ) ) ;
#3987 = CARTESIAN_POINT ( 'NONE',  ( -154.3824083646099439, -184.2938272943107449, 58.62277379824867296 ) ) ;
#3988 = CARTESIAN_POINT ( 'NONE',  ( -154.3824083646099439, -190.5584106276440650, 58.62277379824867296 ) ) ;
#3989 = VERTEX_POINT ( 'NONE', #11873 ) ;
#3990 = CARTESIAN_POINT ( 'NONE',  ( -157.2955611005346270, -175.7084106276440707, 57.67623309621198047 ) ) ;
#3991 = CARTESIAN_POINT ( 'NONE',  ( 10.61292492956169475, 108.6005711365770026, 0.7156557588857267449 ) ) ;
#3992 = ORIENTED_EDGE ( 'NONE', *, *, #4494, .F. ) ;
#3993 = CARTESIAN_POINT ( 'NONE',  ( 47.43856463449117200, 148.7651871740939953, 32.77220824515698183 ) ) ;
#3994 = CARTESIAN_POINT ( 'NONE',  ( 43.01140435219951286, 156.8651871740940180, 38.86567161673127657 ) ) ;
#3995 = CARTESIAN_POINT ( 'NONE',  ( 38.58424406990786082, 105.3797705074273239, 34.21067981925357060 ) ) ;
#3996 = ORIENTED_EDGE ( 'NONE', *, *, #11008, .T. ) ;
#3997 = ORIENTED_EDGE ( 'NONE', *, *, #7265, .T. ) ;
#3998 = CARTESIAN_POINT ( 'NONE',  ( 62.17156016504299032, 99.21662021101468554, 6.584824431686855384 ) ) ;
#3999 = EDGE_LOOP ( 'NONE', ( #6371, #11578, #9584, #16256 ) ) ;
#4000 = CARTESIAN_POINT ( 'NONE',  ( 131.9510975077307933, 193.6375880255003779, 14.00000000000001776 ) ) ;
#4001 = CARTESIAN_POINT ( 'NONE',  ( 41.64333658814960870, 144.7151871740940123, 38.42115945441014446 ) ) ;
#4002 = CARTESIAN_POINT ( 'NONE',  ( 47.05648932407426344, 104.5104996726487485, 31.27175355779120025 ) ) ;
#4003 = CARTESIAN_POINT ( 'NONE',  ( 66.76198117565915879, 95.25264312590786631, -0.5179092472497510702 ) ) ;
#4004 = CARTESIAN_POINT ( 'NONE',  ( -151.4692556286853176, -162.8130981290893260, 59.65701158161632378 ) ) ;
#4005 = CARTESIAN_POINT ( 'NONE',  ( -161.4692556286852607, -170.6391397928654499, 46.40781461928724383 ) ) ;
#4006 = CARTESIAN_POINT ( 'NONE',  ( -143.3790856849358306, -159.3630981290893089, 55.53486410454105027 ) ) ;
#4007 = CARTESIAN_POINT ( 'NONE',  ( 43.01140435219957681, 96.53445800887259054, 39.21067981925356349 ) ) ;
#4008 = LINE ( 'NONE', #4219, #19072 ) ;
#4009 = VERTEX_POINT ( 'NONE', #3508 ) ;
#4010 = CARTESIAN_POINT ( 'NONE',  ( 39.42975644700377558, 87.07977050742732672, 31.60846029578754468 ) ) ;
#4011 = CARTESIAN_POINT ( 'NONE',  ( -148.5561028927606344, -161.7938272943107449, 40.69124936498395328 ) ) ;
#4012 = CARTESIAN_POINT ( 'NONE',  ( 46.59305225739526435, 67.91518717409400097, 31.60846029578754468 ) ) ;
#4013 = CARTESIAN_POINT ( 'NONE',  ( 28.88048086162541850, 151.0887240815949895, -10.63664014359656385 ) ) ;
#4014 = CARTESIAN_POINT ( 'NONE',  ( -154.3824083646099439, -193.5584106276440650, 58.62277379824867296 ) ) ;
#4015 = EDGE_LOOP ( 'NONE', ( #11908, #16204 ) ) ;
#4016 = CARTESIAN_POINT ( 'NONE',  ( 42.21948215057687293, 68.11133943119284595, 29.21067981925355994 ) ) ;
#4017 = LINE ( 'NONE', #8986, #10632 ) ;
#4018 = CARTESIAN_POINT ( 'NONE',  ( 39.42975644700377558, 129.6797705074273210, 36.81289934271958941 ) ) ;
#4019 = CARTESIAN_POINT ( 'NONE',  ( 15.82502354501850483, 112.7224674592991818, 9.875206726065272278 ) ) ;
#4020 = EDGE_LOOP ( 'NONE', ( #19518, #2644, #17019, #15348 ) ) ;
#4021 = CARTESIAN_POINT ( 'NONE',  ( 126.8576204525573274, -136.9891397928655010, 67.64809332337412684 ) ) ;
#4022 = VERTEX_POINT ( 'NONE', #20476 ) ;
#4023 = CARTESIAN_POINT ( 'NONE',  ( 45.74753988029933538, 137.3297705074273267, 30.44471234641811819 ) ) ;
#4024 = ADVANCED_FACE ( 'NONE', ( #10232 ), #1627, .T. ) ;
#4025 = CARTESIAN_POINT ( 'NONE',  ( 38.01140435219952707, 110.9344580088725678, 35.83527830041809636 ) ) ;
#4026 = DIRECTION ( 'NONE',  ( 0.000000000000000000, 0.000000000000000000, -1.000000000000000000 ) ) ;
#4027 =( LENGTH_UNIT ( ) NAMED_UNIT ( * ) SI_UNIT ( .MILLI., .METRE. ) );
#4028 = VECTOR ( 'NONE', #18971, 1000.000000000000000 ) ;
#4029 = EDGE_CURVE ( 'NONE', #20969, #10160, #18710, .T. ) ;
#4030 = CARTESIAN_POINT ( 'NONE',  ( 40.27526882409969033, 101.6651871740940152, 30.44471234641811819 ) ) ;
#4031 = CARTESIAN_POINT ( 'NONE',  ( 44.55648932407425633, 74.81049967264874567, 29.45539723777780239 ) ) ;
#4032 = DIRECTION ( 'NONE',  ( 0.000000000000000000, 0.000000000000000000, 1.000000000000000000 ) ) ;
#4033 = CARTESIAN_POINT ( 'NONE',  ( -141.4692556286852891, -156.0630981290892976, 49.65701158161630957 ) ) ;
#4034 = DIRECTION ( 'NONE',  ( 1.000000000000000000, 0.000000000000000000, 0.000000000000000000 ) ) ;
#4035 = LINE ( 'NONE', #17574, #9321 ) ;
#4036 = CARTESIAN_POINT ( 'NONE',  ( 43.01140435219951286, 129.5344580088726048, 39.46799094044489209 ) ) ;
#4037 = CARTESIAN_POINT ( 'NONE',  ( 44.37947211624943833, 110.4797705074273324, 30.00020018409699318 ) ) ;
#4038 = CARTESIAN_POINT ( 'NONE',  ( 37.44377528459369131, 147.6348322250013894, 2.699600794211013621 ) ) ;
#4039 = CARTESIAN_POINT ( 'NONE',  ( -148.5561028927606344, -189.9938272943107336, 58.62277379824867296 ) ) ;
#4040 = CARTESIAN_POINT ( 'NONE',  ( 39.42975644700377558, 104.8151871740939924, 31.60846029578754468 ) ) ;
#4041 = FACE_OUTER_BOUND ( 'NONE', #14824, .T. ) ;
#4042 = ORIENTED_EDGE ( 'NONE', *, *, #17003, .T. ) ;
#4043 = CARTESIAN_POINT ( 'NONE',  ( 38.96631938032478359, 88.01049967264874851, 37.14960608071593384 ) ) ;
#4044 = CARTESIAN_POINT ( 'NONE',  ( 77.15313604554262383, 122.4041478163663612, -8.494263314424808087 ) ) ;
#4045 = CARTESIAN_POINT ( 'NONE',  ( 68.29827362630597065, 132.3882971431532383, 5.156253003121209488 ) ) ;
#4046 = DIRECTION ( 'NONE',  ( 0.000000000000000000, 1.000000000000000000, 0.000000000000000000 ) ) ;
#4047 = CARTESIAN_POINT ( 'NONE',  ( 44.37947211624943833, 76.27977050742731535, 38.42115945441014446 ) ) ;
#4048 = ORIENTED_EDGE ( 'NONE', *, *, #16598, .T. ) ;
#4049 = EDGE_LOOP ( 'NONE', ( #10376, #18796, #8509, #20618 ) ) ;
#4050 =( BOUNDED_CURVE ( )  B_SPLINE_CURVE ( 2, ( #5250, #3381, #17565, #2472, #12174, #15805, #718, #7449, #10752, #15912, #14154, #20889, #822 ),
 .UNSPECIFIED., .F., .F. ) 
 B_SPLINE_CURVE_WITH_KNOTS ( ( 3, 2, 2, 2, 2, 2, 3 ),
 ( 0.03676470588235294240, 0.03823529411764706176, 0.04117647058823529355, 0.04411764705882353227, 0.04705882352941176405, 0.05000000000000000278, 0.05147058823529411520 ),
 .UNSPECIFIED. ) 
 CURVE ( )  GEOMETRIC_REPRESENTATION_ITEM ( )  RATIONAL_B_SPLINE_CURVE ( ( 0.9755282581475768211, 0.9755282581475768211, 1.000000000000000000, 0.9510565162951535312, 1.000000000000000000, 0.9510565162951535312, 1.000000000000000000, 0.9510565162951535312, 1.000000000000000000, 0.9510565162951535312, 1.000000000000000000, 0.9755282581475768211, 0.9755282581475767101 ) ) 
 REPRESENTATION_ITEM ( '' )  );
#4051 = DIRECTION ( 'NONE',  ( 0.8302490056034136368, 0.5573926701119623628, 0.000000000000000000 ) ) ;
#4052 = CARTESIAN_POINT ( 'NONE',  ( 48.01140435219951996, 116.2104996726487371, 34.21067981925357060 ) ) ;
#4054 = CARTESIAN_POINT ( 'NONE',  ( 25.98494354700934750, 90.29984025740714060, -5.084945496952688160 ) ) ;
#4053 = CARTESIAN_POINT ( 'NONE',  ( 40.27526882409969033, 75.56518717409399244, 37.97664729208901946 ) ) ;
#4055 = CARTESIAN_POINT ( 'NONE',  ( -142.0420953463935803, -174.5438272943107165, 52.72008163687743831 ) ) ;
#4056 = CARTESIAN_POINT ( 'NONE',  ( 19.13088699441526686, 95.37848931739559077, 15.19637875606281341 ) ) ;
#4057 = CARTESIAN_POINT ( 'NONE',  ( -148.3790856849358306, -185.4630981290893033, 40.14644641866477315 ) ) ;
#4058 = CYLINDRICAL_SURFACE ( 'NONE', #16691, 4.999999999999997335 ) ;
#4059 = DIRECTION ( 'NONE',  ( -0.9949940778855791423, -0.09993390301907582873, 0.000000000000000000 ) ) ;
#4060 = CARTESIAN_POINT ( 'NONE',  ( 46.59305225739526435, 143.1797705074273210, 31.60846029578754468 ) ) ;
#4061 = CARTESIAN_POINT ( 'NONE',  ( 73.49404125747247463, 104.1488224428393039, 5.120290292223307560 ) ) ;
#4062 = CARTESIAN_POINT ( 'NONE',  ( 45.74753988029934249, 136.1651871740939725, 37.97664729208901235 ) ) ;
#4063 = EDGE_CURVE ( 'NONE', #20212, #10776, #15071, .T. ) ;
#4064 = PLANE ( 'NONE',  #13238 ) ;
#4065 = CARTESIAN_POINT ( 'NONE',  ( -151.4692556286852891, -169.4084106276440593, 59.56931450028537256 ) ) ;
#4066 = LINE ( 'NONE', #21045, #18173 ) ;
#4067 = EDGE_CURVE ( 'NONE', #18469, #16234, #5049, .T. ) ;
#4068 = LINE ( 'NONE', #759, #7828 ) ;
#4069 = CARTESIAN_POINT ( 'NONE',  ( 50.02529374262071826, 147.3041493969045064, 10.19957357710909207 ) ) ;
#4070 = CYLINDRICAL_SURFACE ( 'NONE', #12334, 4.999999999999997335 ) ;
#4071 = CARTESIAN_POINT ( 'NONE',  ( 38.58424406990784661, 113.9651871740940123, 32.77220824515698183 ) ) ;
#4072 = ORIENTED_EDGE ( 'NONE', *, *, #9917, .T. ) ;
#4073 = CARTESIAN_POINT ( 'NONE',  ( -159.5594255724347761, -160.2630981290893146, 55.53486410454104316 ) ) ;
#4074 = ORIENTED_EDGE ( 'NONE', *, *, #5608, .F. ) ;
#4075 = CARTESIAN_POINT ( 'NONE',  ( 38.01140435219951996, 95.93445800887258201, 35.83527830041810347 ) ) ;
#4076 = CARTESIAN_POINT ( 'NONE',  ( 46.59305225739526435, 148.5797705074273267, 36.81289934271958941 ) ) ;
#4077 = APPLICATION_CONTEXT ( 'automotive_design' ) ;
#4078 = CARTESIAN_POINT ( 'NONE',  ( 44.55648932407425633, 152.8104996726487457, 29.45539723777780239 ) ) ;
#4080 = CARTESIAN_POINT ( 'NONE',  ( 67.81612255856859406, 106.6615363072494915, -6.791355845220972576 ) ) ;
#4079 = CARTESIAN_POINT ( 'NONE',  ( 45.74753988029933538, 103.1651871740940010, 37.97664729208901946 ) ) ;
#4081 = CARTESIAN_POINT ( 'NONE',  ( 38.96631938032478359, 72.41049967264873999, 31.27175355779120025 ) ) ;
#4083 = CARTESIAN_POINT ( 'NONE',  ( 44.55648932407425633, 147.6844580088725820, 38.96596240072933170 ) ) ;
#4082 = LINE ( 'NONE', #16079, #10825 ) ;
#4084 = CARTESIAN_POINT ( 'NONE',  ( 116.4417310231185780, -136.9891397928655010, 30.00000000000000000 ) ) ;
#4085 = VECTOR ( 'NONE', #8189, 1000.000000000000114 ) ;
#4086 = CARTESIAN_POINT ( 'NONE',  ( 147.8787791192428074, -126.9891397928655010, -9.657011581616311346 ) ) ;
#4087 = CARTESIAN_POINT ( 'NONE',  ( 44.37947211624943833, 68.21518717409399812, 30.00020018409699318 ) ) ;
#4088 = CARTESIAN_POINT ( 'NONE',  ( 38.01140435219952707, 63.71049967264874425, 34.21067981925357060 ) ) ;
#4089 = CARTESIAN_POINT ( 'NONE',  ( -143.8425227516148084, -177.0938272943107279, 44.11586579668791330 ) ) ;
#4090 = CARTESIAN_POINT ( 'NONE',  ( -159.0959885057557983, -194.4584106276440423, 44.11586579668791330 ) ) ;
#4091 = ORIENTED_EDGE ( 'NONE', *, *, #9801, .T. ) ;
#4092 = CARTESIAN_POINT ( 'NONE',  ( -142.0420953463935803, -180.5084106276440536, 46.59394152635518793 ) ) ;
#4093 = CARTESIAN_POINT ( 'NONE',  ( 33.74677389505396263, 86.86730044589080535, -0.3555069876874490942 ) ) ;
#4094 = ORIENTED_EDGE ( 'NONE', *, *, #8231, .T. ) ;
#4095 = CARTESIAN_POINT ( 'NONE',  ( 43.01140435219951286, 141.8651871740940180, 38.86567161673127657 ) ) ;
#4096 = CARTESIAN_POINT ( 'NONE',  ( 40.27526882409969744, 108.8297705074273125, 37.97664729208901235 ) ) ;
#4097 = ORIENTED_EDGE ( 'NONE', *, *, #3754, .T. ) ;
#4098 = VERTEX_POINT ( 'NONE', #10882 ) ;
#4099 = AXIS2_PLACEMENT_3D ( 'NONE', #10030, #8156, #14861 ) ;
#4100 = CARTESIAN_POINT ( 'NONE',  ( 22.56676867748217674, 139.3294883087844198, 3.013676707730225779 ) ) ;
#4101 = VECTOR ( 'NONE', #5859, 1000.000000000000000 ) ;
#4102 = VERTEX_POINT ( 'NONE', #15929 ) ;
#4103 = EDGE_CURVE ( 'NONE', #19572, #3065, #12867, .T. ) ;
#4104 = LINE ( 'NONE', #12590, #16410 ) ;
#4105 = CARTESIAN_POINT ( 'NONE',  ( 44.37947211624943833, 139.0151871740939953, 38.42115945441014446 ) ) ;
#4106 = CARTESIAN_POINT ( 'NONE',  ( 43.01140435219951286, 100.4604996726487656, 39.46799094044489209 ) ) ;
#4107 = CARTESIAN_POINT ( 'NONE',  ( 76.92284642892752800, 124.5854180935290714, 5.434424407683230207 ) ) ;
#4108 = CARTESIAN_POINT ( 'NONE',  ( -148.3790856849358306, -179.4630981290893033, 40.14644641866477315 ) ) ;
#4109 = CARTESIAN_POINT ( 'NONE',  ( -141.4692556286852891, -174.8391397928654669, 46.40781461928724383 ) ) ;
#4110 = AXIS2_PLACEMENT_3D ( 'NONE', #21112, #19234, #13938 ) ;
#4111 = CARTESIAN_POINT ( 'NONE',  ( 46.10157429594899270, 158.6604996726487116, 29.95742577749336988 ) ) ;
#4112 = CARTESIAN_POINT ( 'NONE',  ( 38.01140435219952707, 143.6344580088725706, 32.58608133808903773 ) ) ;
#4113 = DIRECTION ( 'NONE',  ( 0.000000000000000000, -1.000000000000000000, 0.000000000000000000 ) ) ;
#4114 = ORIENTED_EDGE ( 'NONE', *, *, #19283, .F. ) ;
#4115 = CARTESIAN_POINT ( 'NONE',  ( 39.42975644700377558, 81.67977050742732104, 36.81289934271958941 ) ) ;
#4116 = CARTESIAN_POINT ( 'NONE',  ( -143.8425227516148084, -162.6938272943107222, 55.19815736654470584 ) ) ;
#4117 = CARTESIAN_POINT ( 'NONE',  ( 39.42975644700377558, 65.81518717409400665, 31.60846029578754468 ) ) ;
#4118 = CARTESIAN_POINT ( 'NONE',  ( 26.28921445626723852, 149.7786157371718616, -3.732453678475698311 ) ) ;
#4119 = CARTESIAN_POINT ( 'NONE',  ( -159.0959885057557983, -191.4584106276440423, 44.11586579668791330 ) ) ;
#4120 = EDGE_LOOP ( 'NONE', ( #9807, #20346, #10050, #6259 ) ) ;
#4121 = EDGE_CURVE ( 'NONE', #10985, #711, #11193, .T. ) ;
#4122 = CARTESIAN_POINT ( 'NONE',  ( 43.80332655382220253, 85.95757658655229250, 29.21067981925356705 ) ) ;
#4123 = CARTESIAN_POINT ( 'NONE',  ( 173.3794444120442506, -34.13255853780189142, 5.000000000000018652 ) ) ;
#4124 = CARTESIAN_POINT ( 'NONE',  ( 41.64333658814960870, 137.7797705074273154, 30.00020018409699318 ) ) ;
#4125 = CARTESIAN_POINT ( 'NONE',  ( 16.85323768375146614, 130.1535925207217588, 10.57871716905499682 ) ) ;
#4126 = VERTEX_POINT ( 'NONE', #7691 ) ;
#4127 = LINE ( 'NONE', #9752, #21365 ) ;
#4128 = ORIENTED_EDGE ( 'NONE', *, *, #10231, .T. ) ;
#4129 = AXIS2_PLACEMENT_3D ( 'NONE', #5886, #2474, #12284 ) ;
#4130 = CARTESIAN_POINT ( 'NONE',  ( 38.58424406990784661, 126.5297705074272727, 35.64915139335016647 ) ) ;
#4131 = CARTESIAN_POINT ( 'NONE',  ( 47.05648932407426344, 109.9104996726487400, 37.14960608071593384 ) ) ;
#4132 = LINE ( 'NONE', #10866, #7747 ) ;
#4133 = LINE ( 'NONE', #19337, #2364 ) ;
#4134 = DIRECTION ( 'NONE',  ( 0.000000000000000000, 0.000000000000000000, 1.000000000000000000 ) ) ;
#4135 = CARTESIAN_POINT ( 'NONE',  ( -141.4692556286852891, -191.9130981290892919, 46.40781461928724383 ) ) ;
#4136 = CIRCLE ( 'NONE', #4292, 10.00000000000000888 ) ;
#4137 = CARTESIAN_POINT ( 'NONE',  ( 40.27526882409969033, 99.56518717409400665, 37.97664729208901946 ) ) ;
#4138 = CARTESIAN_POINT ( 'NONE',  ( -176.9699209214867608, -126.9891397928655010, -35.00000000000000000 ) ) ;
#4139 = CARTESIAN_POINT ( 'NONE',  ( 44.55648932407425633, 124.6104996726487428, 38.96596240072933170 ) ) ;
#4140 = CARTESIAN_POINT ( 'NONE',  ( -155.5590433672037989, -155.1145756620584564, 40.47124192889010885 ) ) ;
#4141 = SHAPE_DEFINITION_REPRESENTATION ( #21024, #13805 ) ;
#4142 = CARTESIAN_POINT ( 'NONE',  ( 48.01140435219951996, 130.2844580088725763, 34.21067981925357060 ) ) ;
#4143 = CARTESIAN_POINT ( 'NONE',  ( 47.43856463449117200, 110.0297705074273296, 32.77220824515698183 ) ) ;
#4144 = CARTESIAN_POINT ( 'NONE',  ( 55.43026649837064213, 94.49908577724413306, 5.913859291446645905 ) ) ;
#4145 = CARTESIAN_POINT ( 'NONE',  ( 116.4417310231185780, -126.9891397928655010, 49.65701158161629536 ) ) ;
#4146 = CARTESIAN_POINT ( 'NONE',  ( 46.59305225739526435, 94.31518717409399244, 36.81289934271958941 ) ) ;
#4147 = VECTOR ( 'NONE', #18159, 1000.000000000000114 ) ;
#4148 = CARTESIAN_POINT ( 'NONE',  ( 41.46631938032478359, 91.31049967264874567, 38.96596240072933170 ) ) ;
#4149 = EDGE_CURVE ( 'NONE', #18306, #21732, #21020, .T. ) ;
#4150 = VERTEX_POINT ( 'NONE', #9231 ) ;
#4151 = EDGE_CURVE ( 'NONE', #14439, #5159, #6099, .T. ) ;
#4152 = DIRECTION ( 'NONE',  ( -0.9385982292947088190, -0.3450121214752274179, 2.040824802394967185E-16 ) ) ;
#4153 = CARTESIAN_POINT ( 'NONE',  ( 75.16956835342354282, 131.6452004531123805, 5.196376467030073165 ) ) ;
#4154 = CARTESIAN_POINT ( 'NONE',  ( 44.86974823489592978, 148.0457227541334362, 10.98970740178311090 ) ) ;
#4155 = DIRECTION ( 'NONE',  ( -0.000000000000000000, 1.000000000000000000, -0.000000000000000000 ) ) ;
#4156 = CARTESIAN_POINT ( 'NONE',  ( 40.27526882409969744, 77.92977050742732104, 30.44471234641812174 ) ) ;
#4157 = ORIENTED_EDGE ( 'NONE', *, *, #6919, .F. ) ;
#4158 = ORIENTED_EDGE ( 'NONE', *, *, #17674, .F. ) ;
#4159 = CARTESIAN_POINT ( 'NONE',  ( 44.37947211624943833, 157.2797705074273438, 38.42115945441014446 ) ) ;
#4160 = FACE_BOUND ( 'NONE', #14959, .T. ) ;
#4161 = COLOUR_RGB ( '', 0.08235294, 0.09019608, 0.10196078) ;
#4162 = CARTESIAN_POINT ( 'NONE',  ( 46.10157429594899270, 122.6604996726487542, 29.95742577749337343 ) ) ;
#4164 = CARTESIAN_POINT ( 'NONE',  ( 75.16838608161717161, 131.4143534805274101, -0.7992312111982662337 ) ) ;
#4163 = CARTESIAN_POINT ( 'NONE',  ( 40.27526882409969033, 74.66518717409397254, 30.44471234641811819 ) ) ;
#4165 = CARTESIAN_POINT ( 'NONE',  ( -143.8425227516148084, -174.6938272943107506, 55.19815736654470584 ) ) ;
#4166 = CARTESIAN_POINT ( 'NONE',  ( 38.54497605562327323, 85.96704844161884296, 14.48200433579215662 ) ) ;
#4167 = CARTESIAN_POINT ( 'NONE',  ( -157.6495955161842062, -184.1130981290893089, 58.16351966513671812 ) ) ;
#4168 = CARTESIAN_POINT ( 'NONE',  ( 151.4773229304660731, 84.89323405393692212, 4.000000000000021316 ) ) ;
#4169 = CARTESIAN_POINT ( 'NONE',  ( 47.05648932407426344, 157.5844580088725877, 31.27175355779120025 ) ) ;
#4170 = CARTESIAN_POINT ( 'NONE',  ( 47.43856463449117200, 139.7297705074273324, 35.64915139335016647 ) ) ;
#4171 = CARTESIAN_POINT ( 'NONE',  ( 66.79148812173782801, 144.6461433805978061, 3.691718863876278345 ) ) ;
#4172 = CARTESIAN_POINT ( 'NONE',  ( 45.74753988029934249, 127.1651871740939725, 37.97664729208901235 ) ) ;
#4173 = EDGE_CURVE ( 'NONE', #18391, #12691, #19038, .T. ) ;
#4174 = CARTESIAN_POINT ( 'NONE',  ( 44.55648932407425633, 136.6104996726487286, 38.96596240072933170 ) ) ;
#4175 = CARTESIAN_POINT ( 'NONE',  ( -143.8425227516148084, -168.9584106276440423, 55.19815736654470584 ) ) ;
#4176 = CARTESIAN_POINT ( 'NONE',  ( 44.82204965540741171, 59.43124467221783647, 30.14400234367970910 ) ) ;
#4177 = CARTESIAN_POINT ( 'NONE',  ( 134.6380592378700101, 268.5785371414991687, -19.99999999999997868 ) ) ;
#4178 = CARTESIAN_POINT ( 'NONE',  ( 69.49514557983670215, 129.8286863358667347, 11.27102936561352742 ) ) ;
#4179 = CARTESIAN_POINT ( 'NONE',  ( 39.42975644700377558, 107.8151871740939924, 31.60846029578754468 ) ) ;
#4180 =( BOUNDED_CURVE ( )  B_SPLINE_CURVE ( 2, ( #734, #19352, #4148, #15927, #839, #7573, #21018, #12630, #4250, #10976, #14385, #14926, #6452 ),
 .UNSPECIFIED., .F., .T. ) 
 B_SPLINE_CURVE_WITH_KNOTS ( ( 3, 2, 2, 2, 2, 2, 3 ),
 ( 0.6691176470588234837, 0.6705882352941175961, 0.6735294117647059320, 0.6764705882352941568, 0.6794117647058823817, 0.6823529411764706065, 0.6838235294117647189 ),
 .UNSPECIFIED. ) 
 CURVE ( )  GEOMETRIC_REPRESENTATION_ITEM ( )  RATIONAL_B_SPLINE_CURVE ( ( 0.9755282581475768211, 0.9755282581475768211, 1.000000000000000000, 0.9510565162951535312, 1.000000000000000000, 0.9510565162951535312, 1.000000000000000000, 0.9510565162951535312, 1.000000000000000000, 0.9510565162951535312, 1.000000000000000000, 0.9755282581475768211, 0.9755282581475768211 ) ) 
 REPRESENTATION_ITEM ( '' )  );
#4181 = ORIENTED_EDGE ( 'NONE', *, *, #7813, .T. ) ;
#4182 = CARTESIAN_POINT ( 'NONE',  ( -141.4692556286852891, -157.1391397928654783, 52.90620854394536821 ) ) ;
#4183 = VERTEX_POINT ( 'NONE', #2168 ) ;
#4184 = CARTESIAN_POINT ( 'NONE',  ( 46.10157429594899270, 96.83445800887255928, 38.46393386101376421 ) ) ;
#4185 = CARTESIAN_POINT ( 'NONE',  ( 41.64333658814960870, 149.7797705074273154, 30.00020018409699318 ) ) ;
#4186 = CARTESIAN_POINT ( 'NONE',  ( 38.96631938032478359, 150.4104996726487400, 31.27175355779120025 ) ) ;
#4188 = CARTESIAN_POINT ( 'NONE',  ( 70.72621728061167801, 115.1542034346632875, -7.148670959876664455 ) ) ;
#4187 = CARTESIAN_POINT ( 'NONE',  ( 38.58424406990784661, 110.9651871740940123, 32.77220824515698183 ) ) ;
#4189 = CARTESIAN_POINT ( 'NONE',  ( 38.01140435219951996, 60.56049967264873146, 32.58608133808903773 ) ) ;
#4190 = DIRECTION ( 'NONE',  ( 0.000000000000000000, 1.000000000000000000, 0.000000000000000000 ) ) ;
#4191 = CARTESIAN_POINT ( 'NONE',  ( 43.01140435219951996, 10.71049967264875491, 34.21067981925357060 ) ) ;
#4192 = AXIS2_PLACEMENT_3D ( 'NONE', #955, #3044, #7699 ) ;
#4193 = CARTESIAN_POINT ( 'NONE',  ( 43.01140435219951286, 81.53445800887257633, 39.21067981925356349 ) ) ;
#4194 = CARTESIAN_POINT ( 'NONE',  ( 83.67254549292280785, -61.68114226949890622, 20.00000000000001776 ) ) ;
#4195 = CARTESIAN_POINT ( 'NONE',  ( 51.60797029699607918, 86.77139250312444574, -6.946567135388369785 ) ) ;
#4196 = CARTESIAN_POINT ( 'NONE',  ( 151.4773229304660731, 84.89323405393692212, 4.000000000000021316 ) ) ;
#4197 = CARTESIAN_POINT ( 'NONE',  ( -148.5561028927606344, -168.9938272943107336, 58.62277379824867296 ) ) ;
#4198 = DIRECTION ( 'NONE',  ( -0.000000000000000000, -0.000000000000000000, 1.000000000000000000 ) ) ;
#4199 = ORIENTED_EDGE ( 'NONE', *, *, #8423, .T. ) ;
#4200 = CARTESIAN_POINT ( 'NONE',  ( 57.78537588620154963, 150.8774031240512272, 3.334753224648476788 ) ) ;
#4201 = FILL_AREA_STYLE_COLOUR ( '', #6715 ) ;
#4202 = CARTESIAN_POINT ( 'NONE',  ( 38.58424406990784661, 134.9651871740940123, 32.77220824515698183 ) ) ;
#4203 = CARTESIAN_POINT ( 'NONE',  ( 38.58424406990785371, 93.22977050742731819, 32.77220824515697473 ) ) ;
#4204 = VERTEX_POINT ( 'NONE', #8906 ) ;
#4205 = ORIENTED_EDGE ( 'NONE', *, *, #14991, .T. ) ;
#4206 = CARTESIAN_POINT ( 'NONE',  ( 29.72792815944318789, 144.7825833525567134, 3.370790685444458479 ) ) ;
#4207 = VERTEX_POINT ( 'NONE', #517 ) ;
#4208 = CARTESIAN_POINT ( 'NONE',  ( 43.01140435219951286, 113.0344580088725621, 28.95336869806222779 ) ) ;
#4209 = PRODUCT_RELATED_PRODUCT_CATEGORY ( 'part', '', ( #1501 ) ) ;
#4210 = CARTESIAN_POINT ( 'NONE',  ( 38.01140435219952707, 75.86049967264874283, 35.83527830041809636 ) ) ;
#4211 = CARTESIAN_POINT ( 'NONE',  ( 46.59305225739526435, 74.17977050742732104, 31.60846029578754468 ) ) ;
#4212 = CARTESIAN_POINT ( 'NONE',  ( 41.64333658814960870, 132.7151871740940123, 38.42115945441014446 ) ) ;
#4213 = CARTESIAN_POINT ( 'NONE',  ( 38.01140435219951996, 93.86049967264874283, 35.83527830041810347 ) ) ;
#4214 = CARTESIAN_POINT ( 'NONE',  ( 48.17517050666977241, 153.7480039124125994, 4.005852979123367241 ) ) ;
#4215 = CARTESIAN_POINT ( 'NONE',  ( 38.51754685674856660, 95.31395939335972400, 36.42700876960375922 ) ) ;
#4216 = CARTESIAN_POINT ( 'NONE',  ( -161.4692556286852607, -164.6391397928654499, 46.40781461928724383 ) ) ;
#4217 = CARTESIAN_POINT ( 'NONE',  ( 48.01140435219951996, 158.0604996726487173, 35.83527830041809636 ) ) ;
#4218 = DIRECTION ( 'NONE',  ( 0.000000000000000000, -1.000000000000000000, 0.000000000000000000 ) ) ;
#4219 = CARTESIAN_POINT ( 'NONE',  ( 136.0032066456581390, 182.5367998656340944, 34.00000000000001421 ) ) ;
#4220 =( GEOMETRIC_REPRESENTATION_CONTEXT ( 3 ) GLOBAL_UNCERTAINTY_ASSIGNED_CONTEXT ( ( #20336 ) ) GLOBAL_UNIT_ASSIGNED_CONTEXT ( ( #21579, #1843, #6470 ) ) REPRESENTATION_CONTEXT ( 'NONE', 'WORKASPACE' ) );
#4221 = VERTEX_POINT ( 'NONE', #20906 ) ;
#4222 = CARTESIAN_POINT ( 'NONE',  ( 38.58424406990784661, 72.22977050742733240, 32.77220824515698183 ) ) ;
#4223 = CARTESIAN_POINT ( 'NONE',  ( -148.5561028927606344, -164.7938272943107449, 40.69124936498395328 ) ) ;
#4224 = ADVANCED_FACE ( 'NONE', ( #13953 ), #19249, .T. ) ;
#4225 = CARTESIAN_POINT ( 'NONE',  ( 39.42188022582085694, 153.9507182763122159, -10.27990332573616961 ) ) ;
#4226 = CYLINDRICAL_SURFACE ( 'NONE', #7967, 9.999999999999994671 ) ;
#4227 = EDGE_LOOP ( 'NONE', ( #4362, #2305, #1725, #918 ) ) ;
#4228 = CARTESIAN_POINT ( 'NONE',  ( -79.69854755000110913, 605.3054376597395958, -19.99999999999996092 ) ) ;
#4229 = CARTESIAN_POINT ( 'NONE',  ( 39.92123440845005433, 104.3344580088725735, 29.95742577749336988 ) ) ;
#4230 = CARTESIAN_POINT ( 'NONE',  ( 43.01140435219951286, 136.1297705074273381, 38.86567161673127657 ) ) ;
#4231 = EDGE_CURVE ( 'NONE', #10160, #10827, #7575, .T. ) ;
#4232 = EDGE_LOOP ( 'NONE', ( #19120, #18194, #14335, #3347 ) ) ;
#4233 = CARTESIAN_POINT ( 'NONE',  ( 46.10157429594899270, 72.83445800887257349, 38.46393386101375711 ) ) ;
#4234 = ORIENTED_EDGE ( 'NONE', *, *, #13263, .T. ) ;
#4235 = CARTESIAN_POINT ( 'NONE',  ( 38.58424406990786082, 123.3797705074273239, 34.21067981925357060 ) ) ;
#4236 = CARTESIAN_POINT ( 'NONE',  ( 46.10157429594899270, 139.7344580088725934, 29.95742577749336988 ) ) ;
#4237 = CARTESIAN_POINT ( 'NONE',  ( 139.9279279298906147, 262.8829071470229906, -5.999999999999976019 ) ) ;
#4238 = DIRECTION ( 'NONE',  ( -1.000000000000000000, -0.000000000000000000, -0.000000000000000000 ) ) ;
#4239 = CARTESIAN_POINT ( 'NONE',  ( 43.01140435219951996, 158.9604996726487514, 29.21067981925357060 ) ) ;
#4240 = CARTESIAN_POINT ( 'NONE',  ( -141.4692556286852891, -193.1391397928654783, 52.90620854394536821 ) ) ;
#4241 = DIRECTION ( 'NONE',  ( -1.000000000000000000, 0.000000000000000000, 0.000000000000000000 ) ) ;
#4242 = CARTESIAN_POINT ( 'NONE',  ( 43.80332655382220253, 124.5373810949689926, 39.21067981925355639 ) ) ;
#4243 = CARTESIAN_POINT ( 'NONE',  ( -157.6495955161842062, -163.1130981290892805, 58.16351966513671812 ) ) ;
#4244 = EDGE_CURVE ( 'NONE', #14342, #3147, #17903, .T. ) ;
#4245 = CARTESIAN_POINT ( 'NONE',  ( 46.10157429594899270, 133.7344580088725650, 29.95742577749337343 ) ) ;
#4246 = CARTESIAN_POINT ( 'NONE',  ( 38.58424406990784661, 111.2297705074273324, 32.77220824515698183 ) ) ;
#4247 = CARTESIAN_POINT ( 'NONE',  ( 15.40311202476076780, 126.0397005259128065, 8.413886508562818278 ) ) ;
#4248 = CARTESIAN_POINT ( 'NONE',  ( -145.6429501568359797, -188.9438272943106938, 41.63779006702063867 ) ) ;
#4249 = CARTESIAN_POINT ( 'NONE',  ( 41.64333658814960870, 95.51518717409400949, 30.00020018409699318 ) ) ;
#4250 = CARTESIAN_POINT ( 'NONE',  ( 38.96631938032478359, 90.41049967264875420, 31.27175355779120025 ) ) ;
#4251 = ORIENTED_EDGE ( 'NONE', *, *, #3330, .F. ) ;
#4252 = CARTESIAN_POINT ( 'NONE',  ( 47.05648932407426344, 75.98445800887257917, 37.14960608071593384 ) ) ;
#4253 = CARTESIAN_POINT ( 'NONE',  ( 77.22939692449374149, 120.9137088693742044, 5.553548964694690504 ) ) ;
#4254 = CARTESIAN_POINT ( 'NONE',  ( 26.83015598135647295, 142.9878415585355071, 17.22988066553158149 ) ) ;
#4255 = DIRECTION ( 'NONE',  ( -1.000000000000000000, 0.000000000000000000, -0.000000000000000000 ) ) ;
#4256 = CARTESIAN_POINT ( 'NONE',  ( 45.74753988029934249, 74.32977050742731251, 30.44471234641812174 ) ) ;
#4257 = ORIENTED_EDGE ( 'NONE', *, *, #2207, .F. ) ;
#4258 = EDGE_CURVE ( 'NONE', #15220, #21430, #19462, .T. ) ;
#4259 = ORIENTED_EDGE ( 'NONE', *, *, #4577, .T. ) ;
#4260 = CARTESIAN_POINT ( 'NONE',  ( 44.37947211624943833, 158.4797705074273040, 30.00020018409699318 ) ) ;
#4261 = DIRECTION ( 'NONE',  ( -1.000000000000000000, 0.000000000000000000, 0.000000000000000000 ) ) ;
#4262 = CARTESIAN_POINT ( 'NONE',  ( 41.46631938032478359, 118.3104996726487457, 38.96596240072933170 ) ) ;
#4264 = CARTESIAN_POINT ( 'NONE',  ( 76.77449255912956971, 125.0547954796211485, -7.584917068115353267 ) ) ;
#4263 = CARTESIAN_POINT ( 'NONE',  ( 47.43856463449117200, 79.76518717409400949, 32.77220824515698183 ) ) ;
#4265 = CARTESIAN_POINT ( 'NONE',  ( -148.5561028927606344, -171.9938272943107336, 58.62277379824867296 ) ) ;
#4266 = CARTESIAN_POINT ( 'NONE',  ( 42.21854335081802390, 85.68333463812091111, 14.36287948008016890 ) ) ;
#4267 = CARTESIAN_POINT ( 'NONE',  ( -141.4692556286852891, -192.0630981290892976, 49.65701158161630957 ) ) ;
#4268 = FACE_OUTER_BOUND ( 'NONE', #3015, .T. ) ;
#4269 = CARTESIAN_POINT ( 'NONE',  ( 38.96631938032478359, 158.4844580088725934, 31.27175355779120025 ) ) ;
#4270 = CARTESIAN_POINT ( 'NONE',  ( 47.43856463449118621, 145.8797705074273097, 34.21067981925357060 ) ) ;
#4271 = CARTESIAN_POINT ( 'NONE',  ( 8.843693174888816344, 123.0768258502195067, 1.191984145255910787 ) ) ;
#4272 = CARTESIAN_POINT ( 'NONE',  ( 43.01140435219951286, 122.3651871740939896, 29.55568802177586107 ) ) ;
#4273 = CARTESIAN_POINT ( 'NONE',  ( -151.4692556286852891, -160.4084106276440593, 59.56931450028537256 ) ) ;
#4274 = FACE_OUTER_BOUND ( 'NONE', #8740, .T. ) ;
#4275 = CARTESIAN_POINT ( 'NONE',  ( -156.4692903108300186, -155.9898770414735623, 40.99677756761010272 ) ) ;
#4276 = CARTESIAN_POINT ( 'NONE',  ( 65.02109649036992778, 137.6666368931563227, 10.91413209638136728 ) ) ;
#4277 = CARTESIAN_POINT ( 'NONE',  ( 47.43856463449118621, 109.6151871740940038, 34.21067981925357060 ) ) ;
#4278 = EDGE_LOOP ( 'NONE', ( #15239, #11300 ) ) ;
#4279 = LINE ( 'NONE', #4605, #7485 ) ;
#4280 = EDGE_LOOP ( 'NONE', ( #14464, #4432, #12496, #9 ) ) ;
#4281 = CARTESIAN_POINT ( 'NONE',  ( 43.01140435219951286, 93.53445800887257633, 39.46799094044489209 ) ) ;
#4282 = DIRECTION ( 'NONE',  ( 0.000000000000000000, -1.000000000000000000, 0.000000000000000000 ) ) ;
#4283 = ADVANCED_FACE ( 'NONE', ( #16257, #8227, #6228, #19564 ), #18247, .F. ) ;
#4284 = PRODUCT_DEFINITION_SHAPE ( 'NONE', 'NONE',  #20915 ) ;
#4285 = VECTOR ( 'NONE', #17335, 1000.000000000000000 ) ;
#4286 = AXIS2_PLACEMENT_3D ( 'NONE', #11428, #15955, #4377 ) ;
#4288 = CARTESIAN_POINT ( 'NONE',  ( 34.95631105476920197, 146.8486248254830855, -9.410786671241964996 ) ) ;
#4287 = CARTESIAN_POINT ( 'NONE',  ( 39.42975644700377558, 102.4151871740940010, 36.81289934271958941 ) ) ;
#4289 = CARTESIAN_POINT ( 'NONE',  ( 38.96631938032478359, 63.41049967264873999, 31.27175355779120025 ) ) ;
#4291 = CARTESIAN_POINT ( 'NONE',  ( 47.05648932407426344, 60.98445800887257207, 37.14960608071593384 ) ) ;
#4290 = CARTESIAN_POINT ( 'NONE',  ( 45.23316362766301779, 144.8099831305763985, 38.70176206714168643 ) ) ;
#4292 = AXIS2_PLACEMENT_3D ( 'NONE', #10711, #17414, #2319 ) ;
#4293 = CARTESIAN_POINT ( 'NONE',  ( 48.01140435219951996, 146.3604996726487570, 32.58608133808903773 ) ) ;
#4294 = CARTESIAN_POINT ( 'NONE',  ( 43.01140435219951286, 68.36518717409400381, 29.55568802177586463 ) ) ;
#4295 = CARTESIAN_POINT ( 'NONE',  ( 32.31036143884366396, 152.4250368413922274, -10.51794503956956817 ) ) ;
#4296 = DIRECTION ( 'NONE',  ( 0.000000000000000000, 1.000000000000000000, 0.000000000000000000 ) ) ;
#4297 = CARTESIAN_POINT ( 'NONE',  ( -143.8425227516148084, -171.6938272943107222, 55.19815736654470584 ) ) ;
#4298 = CARTESIAN_POINT ( 'NONE',  ( -159.0959885057557983, -181.8584106276440480, 55.19815736654470584 ) ) ;
#4299 = ORIENTED_EDGE ( 'NONE', *, *, #12587, .T. ) ;
#4300 =( BOUNDED_CURVE ( )  B_SPLINE_CURVE ( 2, ( #15303, #5160, #11881, #3515, #1749, #14850, #11769, #6486, #18610, #197, #9806, #13100, #13206 ),
 .UNSPECIFIED., .F., .F. ) 
 B_SPLINE_CURVE_WITH_KNOTS ( ( 3, 2, 2, 2, 2, 2, 3 ),
 ( 0.6250000000000000000, 0.6285714285714285587, 0.6357142857142856762, 0.6428571428571429047, 0.6500000000000000222, 0.6571428571428571397, 0.6607142857142856984 ),
 .UNSPECIFIED. ) 
 CURVE ( )  GEOMETRIC_REPRESENTATION_ITEM ( )  RATIONAL_B_SPLINE_CURVE ( ( 0.9755282581475768211, 0.9755282581475768211, 1.000000000000000000, 0.9510565162951535312, 1.000000000000000000, 0.9510565162951535312, 1.000000000000000000, 0.9510565162951535312, 1.000000000000000000, 0.9510565162951535312, 1.000000000000000000, 0.9755282581475768211, 0.9755282581475768211 ) ) 
 REPRESENTATION_ITEM ( '' )  );
#4301 = CARTESIAN_POINT ( 'NONE',  ( -142.0420953463936087, -168.6584106276440593, 49.65701158161630957 ) ) ;
#4302 = CARTESIAN_POINT ( 'NONE',  ( 9.585575214713108139, 112.1464265272871188, 0.8345760063739874335 ) ) ;
#4303 = EDGE_CURVE ( 'NONE', #20212, #11299, #8375, .T. ) ;
#4304 = ORIENTED_EDGE ( 'NONE', *, *, #7932, .F. ) ;
#4305 = CARTESIAN_POINT ( 'NONE',  ( 45.74753988029933538, 136.1651871740939725, 37.97664729208901946 ) ) ;
#4306 = CARTESIAN_POINT ( 'NONE',  ( 45.74753988029934249, 155.0651871740940067, 30.44471234641812174 ) ) ;
#4307 = CARTESIAN_POINT ( 'NONE',  ( 44.37947211624943833, 94.27977050742731535, 38.42115945441014446 ) ) ;
#4308 = ORIENTED_EDGE ( 'NONE', *, *, #21220, .T. ) ;
#4309 = ORIENTED_EDGE ( 'NONE', *, *, #15936, .T. ) ;
#4310 = CARTESIAN_POINT ( 'NONE',  ( 19.23080508249268661, 135.0620028898917440, 9.799277925644819476 ) ) ;
#4311 = ORIENTED_EDGE ( 'NONE', *, *, #3156, .T. ) ;
#4312 = CARTESIAN_POINT ( 'NONE',  ( 43.01140435219951286, 117.5344580088725621, 39.46799094044489209 ) ) ;
#4313 = FACE_BOUND ( 'NONE', #6310, .T. ) ;
#4314 = CARTESIAN_POINT ( 'NONE',  ( 41.64333658814960870, 75.97977050742731819, 38.42115945441014446 ) ) ;
#4315 = CARTESIAN_POINT ( 'NONE',  ( 43.01140435219951286, 135.8651871740940180, 38.86567161673127657 ) ) ;
#4316 = CARTESIAN_POINT ( 'NONE',  ( 48.01140435219951996, 89.36049967264874283, 32.58608133808903773 ) ) ;
#4317 = CARTESIAN_POINT ( 'NONE',  ( 58.57487293839693621, 150.3975950434478648, 4.362879525569486994 ) ) ;
#4318 = CARTESIAN_POINT ( 'NONE',  ( -120.0322075325610740, -126.9891397928655010, 49.65701158161630957 ) ) ;
#4319 = CARTESIAN_POINT ( 'NONE',  ( -145.2889157411863721, -156.5391397928654840, 41.15050349809590102 ) ) ;
#4320 = CARTESIAN_POINT ( 'NONE',  ( 173.3794444120442506, -126.9891397928655010, -17.64809332337413750 ) ) ;
#4321 = DIRECTION ( 'NONE',  ( 0.000000000000000000, -0.000000000000000000, 1.000000000000000000 ) ) ;
#4322 = DIRECTION ( 'NONE',  ( -0.000000000000000000, 1.000000000000000000, -0.000000000000000000 ) ) ;
#4323 = VERTEX_POINT ( 'NONE', #4574 ) ;
#4324 = CARTESIAN_POINT ( 'NONE',  ( 40.27526882409969033, 78.82977050742731251, 37.97664729208901946 ) ) ;
#4325 = CARTESIAN_POINT ( 'NONE',  ( -148.5561028927606344, -168.9938272943107336, 58.62277379824867296 ) ) ;
#4326 = CARTESIAN_POINT ( 'NONE',  ( 64.59149290518072917, 93.33317027722591774, -7.422718449586769296 ) ) ;
#4327 = DIRECTION ( 'NONE',  ( -0.000000000000000000, -0.000000000000000000, -1.000000000000000000 ) ) ;
#4328 = EDGE_LOOP ( 'NONE', ( #1449, #19360 ) ) ;
#4329 = DIRECTION ( 'NONE',  ( -1.000000000000000000, 0.000000000000000000, 0.000000000000000000 ) ) ;
#4330 = CARTESIAN_POINT ( 'NONE',  ( 165.8083469658213005, 192.9029763258799335, -29.99999999999997868 ) ) ;
#4331 = CARTESIAN_POINT ( 'NONE',  ( 46.59305225739526435, 128.1797705074273210, 31.60846029578754468 ) ) ;
#4332 = EDGE_LOOP ( 'NONE', ( #21563, #20807 ) ) ;
#4333 = CARTESIAN_POINT ( 'NONE',  ( 44.55648932407425633, 87.68445800887258201, 38.96596240072933170 ) ) ;
#4334 = ORIENTED_EDGE ( 'NONE', *, *, #1961, .T. ) ;
#4335 = CARTESIAN_POINT ( 'NONE',  ( 39.42975644700377558, 129.6797705074273210, 36.81289934271958941 ) ) ;
#4336 = CARTESIAN_POINT ( 'NONE',  ( 43.80332655382219542, 139.9575765865523067, 29.21067981925356705 ) ) ;
#4337 = CARTESIAN_POINT ( 'NONE',  ( 38.96631938032478359, 60.08445800887257349, 37.14960608071593384 ) ) ;
#4338 = ADVANCED_FACE ( 'NONE', ( #14716 ), #4459, .T. ) ;
#4339 = CARTESIAN_POINT ( 'NONE',  ( 137.5268905834513191, 193.0332408774651185, 4.000000000000021316 ) ) ;
#4340 = CARTESIAN_POINT ( 'NONE',  ( 39.92123440845005433, 84.23445800887256496, 38.46393386101375711 ) ) ;
#4341 = CARTESIAN_POINT ( 'NONE',  ( -151.4692556286852891, -194.3130981290893260, 39.65701158161630246 ) ) ;
#4342 = CARTESIAN_POINT ( 'NONE',  ( -143.3790856849358306, -186.6891397928654612, 43.77915905869157598 ) ) ;
#4343 = DIRECTION ( 'NONE',  ( -1.140132994654635861E-16, -0.000000000000000000, -1.000000000000000000 ) ) ;
#4344 = CARTESIAN_POINT ( 'NONE',  ( -145.2889157411863721, -162.5130981290893430, 58.16351966513671812 ) ) ;
#4345 = CARTESIAN_POINT ( 'NONE',  ( 43.01140435219951286, 131.0344580088725763, 28.95336869806222779 ) ) ;
#4346 = CARTESIAN_POINT ( 'NONE',  ( 45.74753988029933538, 107.3297705074272983, 30.44471234641811819 ) ) ;
#4347 = CARTESIAN_POINT ( 'NONE',  ( 70.16915148685765757, 112.0176666281686977, 11.98539833154344691 ) ) ;
#4348 = LINE ( 'NONE', #12628, #13097 ) ;
#4349 = CARTESIAN_POINT ( 'NONE',  ( 39.42975644700377558, 92.81518717409399244, 31.60846029578754468 ) ) ;
#4350 = CARTESIAN_POINT ( 'NONE',  ( 180.1254907973641934, 54.87273858953557237, -19.99999999999997868 ) ) ;
#4351 = ORIENTED_EDGE ( 'NONE', *, *, #5830, .F. ) ;
#4352 = CARTESIAN_POINT ( 'NONE',  ( 43.80332655382220253, 128.8836182503284533, 29.21067981925356705 ) ) ;
#4353 = CARTESIAN_POINT ( 'NONE',  ( 32.14050509837299785, 87.44534670509604268, 7.696117750009315195 ) ) ;
#4354 = CARTESIAN_POINT ( 'NONE',  ( 15.16534570839878349, 115.4582699162533288, 15.98979919289822149 ) ) ;
#4355 = CARTESIAN_POINT ( 'NONE',  ( 77.15313604554262383, 122.4041478163663612, -8.494263314424808087 ) ) ;
#4356 = CARTESIAN_POINT ( 'NONE',  ( 40.27526882409969744, 72.82977050742732672, 37.97664729208901235 ) ) ;
#4357 = ORIENTED_EDGE ( 'NONE', *, *, #2133, .F. ) ;
#4358 = VERTEX_POINT ( 'NONE', #9554 ) ;
#4359 = CARTESIAN_POINT ( 'NONE',  ( 45.74753988029933538, 151.4297705074273210, 37.97664729208901946 ) ) ;
#4361 = ADVANCED_FACE ( 'NONE', ( #9878 ), #16578, .T. ) ;
#4360 = CARTESIAN_POINT ( 'NONE',  ( 147.5268905834513475, 193.0332408774651185, 14.00000000000001776 ) ) ;
#4362 = ORIENTED_EDGE ( 'NONE', *, *, #4637, .T. ) ;
#4363 = CARTESIAN_POINT ( 'NONE',  ( 39.92123440845004723, 123.2604996726487201, 29.95742577749337343 ) ) ;
#4365 = CARTESIAN_POINT ( 'NONE',  ( 12.20328755962376199, 134.6477104347696923, -3.418325544530929516 ) ) ;
#4364 = CARTESIAN_POINT ( 'NONE',  ( 47.43856463449118621, 82.61518717409398960, 34.21067981925357060 ) ) ;
#4366 = CARTESIAN_POINT ( 'NONE',  ( -148.5561028927606344, -173.7938272943107165, 40.69124936498395328 ) ) ;
#4367 = CARTESIAN_POINT ( 'NONE',  ( 138.4989748031516967, 208.9305787985672680, -29.99999999999997868 ) ) ;
#4368 = CARTESIAN_POINT ( 'NONE',  ( -157.6495955161842062, -185.0130981290893146, 41.15050349809590102 ) ) ;
#4369 = CARTESIAN_POINT ( 'NONE',  ( -47.86331837773882825, -19.06233958201669765, -19.99999999999997513 ) ) ;
#4370 = CARTESIAN_POINT ( 'NONE',  ( 38.01140435219952707, 149.7844580088725763, 34.21067981925357060 ) ) ;
#4371 = CARTESIAN_POINT ( 'NONE',  ( 46.59305225739526435, 131.1797705074273210, 31.60846029578754468 ) ) ;
#4372 = CARTESIAN_POINT ( 'NONE',  ( 64.81014823317600815, 93.40725510594978687, -1.427111354441281899 ) ) ;
#4373 = CARTESIAN_POINT ( 'NONE',  ( 47.43856463449117911, 121.7651871740939953, 32.77220824515697473 ) ) ;
#4374 = CARTESIAN_POINT ( 'NONE',  ( 47.05648932407426344, 136.9104996726487400, 37.14960608071593384 ) ) ;
#4375 = CYLINDRICAL_SURFACE ( 'NONE', #14133, 4.999999999999997335 ) ;
#4376 = CARTESIAN_POINT ( 'NONE',  ( -161.4692556286853176, -164.4891397928654726, 49.65701158161630957 ) ) ;
#4377 = DIRECTION ( 'NONE',  ( 0.000000000000000000, 0.000000000000000000, 1.000000000000000000 ) ) ;
#4378 = AXIS2_PLACEMENT_3D ( 'NONE', #472, #13589, #10617 ) ;
#4379 = CARTESIAN_POINT ( 'NONE',  ( 15.11992972970532279, 115.2318815533876375, 21.98540506394948224 ) ) ;
#4380 = CARTESIAN_POINT ( 'NONE',  ( 43.80332655382220253, 83.88361825032845331, 29.21067981925356705 ) ) ;
#4381 = CARTESIAN_POINT ( 'NONE',  ( 38.58424406990784661, 104.9651871740940123, 32.77220824515698183 ) ) ;
#4382 = EDGE_CURVE ( 'NONE', #1334, #1240, #7899, .T. ) ;
#4383 = ORIENTED_EDGE ( 'NONE', *, *, #6351, .F. ) ;
#4384 = CARTESIAN_POINT ( 'NONE',  ( -141.4692556286852891, -156.9891397928654726, 49.65701158161630957 ) ) ;
#4385 = ORIENTED_EDGE ( 'NONE', *, *, #10963, .T. ) ;
#4386 = CARTESIAN_POINT ( 'NONE',  ( 38.01140435219951996, 92.63445800887258486, 32.58608133808903773 ) ) ;
#4387 = DIRECTION ( 'NONE',  ( -1.000000000000000000, 0.000000000000000000, 0.000000000000000000 ) ) ;
#4388 = CARTESIAN_POINT ( 'NONE',  ( 43.01140435219951286, 148.4604996726487229, 39.46799094044489209 ) ) ;
#4390 = CARTESIAN_POINT ( 'NONE',  ( 18.53657114080759527, 106.0614633106838909, -4.410498573173142312 ) ) ;
#4389 = CARTESIAN_POINT ( 'NONE',  ( 47.43856463449117200, 106.4651871740939981, 35.64915139335016647 ) ) ;
#4391 = CARTESIAN_POINT ( 'NONE',  ( 43.01140435219951286, 61.46049967264873004, 39.46799094044489209 ) ) ;
#4393 = CARTESIAN_POINT ( 'NONE',  ( -141.4692556286852891, -183.2130981290892748, 52.90620854394536821 ) ) ;
#4392 = FACE_OUTER_BOUND ( 'NONE', #9072, .T. ) ;
#4394 = CARTESIAN_POINT ( 'NONE',  ( 43.01140435219951286, 119.0344580088725621, 29.21067981925356705 ) ) ;
#4395 = CARTESIAN_POINT ( 'NONE',  ( -157.6495955161842062, -187.1130981290893089, 58.16351966513671812 ) ) ;
#4396 = CARTESIAN_POINT ( 'NONE',  ( 43.80332655382220253, 146.8836182503284817, 29.21067981925356705 ) ) ;
#4397 = CARTESIAN_POINT ( 'NONE',  ( 40.27526882409969033, 71.66518717409400097, 30.44471234641811819 ) ) ;
#4398 = CARTESIAN_POINT ( 'NONE',  ( 64.11693453485118255, 146.8606268255622638, -2.422805558527139080 ) ) ;
#4399 = CARTESIAN_POINT ( 'NONE',  ( 41.46631938032478359, 115.3104996726487599, 38.96596240072933170 ) ) ;
#4400 = CIRCLE ( 'NONE', #3713, 9.999999999999994671 ) ;
#4401 = CARTESIAN_POINT ( 'NONE',  ( -160.8964159109769696, -172.7438272943107336, 52.72008163687743121 ) ) ;
#4402 = CARTESIAN_POINT ( 'NONE',  ( -145.6429501568359797, -183.2084106276440423, 41.63779006702063867 ) ) ;
#4403 = ORIENTED_EDGE ( 'NONE', *, *, #8525, .T. ) ;
#4404 = CARTESIAN_POINT ( 'NONE',  ( -159.0959885057557983, -167.4584106276440423, 44.11586579668791330 ) ) ;
#4405 = CARTESIAN_POINT ( 'NONE',  ( 13.97286934428321103, 138.1879231288898495, 15.71574578848041881 ) ) ;
#4406 = EDGE_LOOP ( 'NONE', ( #468, #5418 ) ) ;
#4407 = CARTESIAN_POINT ( 'NONE',  ( 47.43856463449118621, 136.6151871740940180, 34.21067981925357060 ) ) ;
#4408 = EDGE_CURVE ( 'NONE', #10633, #13533, #16149, .T. ) ;
#4409 = CARTESIAN_POINT ( 'NONE',  ( 46.59305225739526435, 154.3151871740940067, 36.81289934271958941 ) ) ;
#4410 = CARTESIAN_POINT ( 'NONE',  ( 47.43856463449117911, 91.72977050742730398, 35.64915139335015937 ) ) ;
#4411 = ORIENTED_EDGE ( 'NONE', *, *, #7925, .F. ) ;
#4412 = ORIENTED_EDGE ( 'NONE', *, *, #7246, .T. ) ;
#4413 = FILL_AREA_STYLE ('',( #19520 ) ) ;
#4414 = ORIENTED_EDGE ( 'NONE', *, *, #12977, .F. ) ;
#4415 = CARTESIAN_POINT ( 'NONE',  ( 41.46631938032478359, 117.3844580088725849, 38.96596240072933170 ) ) ;
#4416 = LINE ( 'NONE', #13242, #10438 ) ;
#4417 = AXIS2_PLACEMENT_3D ( 'NONE', #3329, #1344, #4753 ) ;
#4418 = CARTESIAN_POINT ( 'NONE',  ( 40.27526882409969033, 74.92977050742732104, 30.44471234641811819 ) ) ;
#4419 = CARTESIAN_POINT ( 'NONE',  ( 46.59305225739526435, 130.9151871740940010, 31.60846029578754468 ) ) ;
#4420 = CARTESIAN_POINT ( 'NONE',  ( 48.01140435219951996, 95.36049967264872862, 32.58608133808903773 ) ) ;
#4421 = CARTESIAN_POINT ( 'NONE',  ( 75.80354157443048280, 110.0810758630161672, 5.910575721798123183 ) ) ;
#4422 = CARTESIAN_POINT ( 'NONE',  ( 43.01140435219951286, 94.90707761860558378, 39.21067981925356349 ) ) ;
#4423 = CARTESIAN_POINT ( 'NONE',  ( -148.3790856849358306, -165.3891397928654499, 40.14644641866477315 ) ) ;
#4424 =( BOUNDED_CURVE ( )  B_SPLINE_CURVE ( 2, ( #17544, #2561, #10948, #12487, #20762, #9194, #8975, #4112, #585, #5654, #17437, #14132, #12374 ),
 .UNSPECIFIED., .F., .T. ) 
 B_SPLINE_CURVE_WITH_KNOTS ( ( 3, 2, 2, 2, 2, 2, 3 ),
 ( 0.1397058823529411797, 0.1411764705882352922, 0.1441176470588235170, 0.1470588235294117696, 0.1499999999999999944, 0.1529411764705882470, 0.1544117647058823595 ),
 .UNSPECIFIED. ) 
 CURVE ( )  GEOMETRIC_REPRESENTATION_ITEM ( )  RATIONAL_B_SPLINE_CURVE ( ( 0.9755282581475768211, 0.9755282581475768211, 1.000000000000000000, 0.9510565162951535312, 1.000000000000000000, 0.9510565162951535312, 1.000000000000000000, 0.9510565162951535312, 1.000000000000000000, 0.9510565162951535312, 1.000000000000000000, 0.9755282581475768211, 0.9755282581475768211 ) ) 
 REPRESENTATION_ITEM ( '' )  );
#4425 = CARTESIAN_POINT ( 'NONE',  ( 43.01140435219952707, 144.9070776186055696, 39.21067981925356349 ) ) ;
#4426 = EDGE_LOOP ( 'NONE', ( #4992, #11145, #923, #21458 ) ) ;
#4427 = CARTESIAN_POINT ( 'NONE',  ( 43.01140435219951286, 76.12977050742732388, 38.86567161673127657 ) ) ;
#4428 = CARTESIAN_POINT ( 'NONE',  ( -142.0420953463936087, -156.3938272943107393, 49.65701158161630957 ) ) ;
#4429 = CARTESIAN_POINT ( 'NONE',  ( 17.14282613681034917, 97.48634091255654255, 8.291567264837656381 ) ) ;
#4430 = CARTESIAN_POINT ( 'NONE',  ( -142.0420953463935803, -186.5084106276440536, 46.59394152635518793 ) ) ;
#4431 = AXIS2_PLACEMENT_3D ( 'NONE', #19436, #1246, #11054 ) ;
#4432 = ORIENTED_EDGE ( 'NONE', *, *, #10310, .F. ) ;
#4433 = PLANE ( 'NONE',  #4787 ) ;
#4434 = VECTOR ( 'NONE', #16810, 1000.000000000000114 ) ;
#4435 = CARTESIAN_POINT ( 'NONE',  ( -156.4692903108300186, -155.9898770414735623, 40.99677756761010272 ) ) ;
#4436 = CARTESIAN_POINT ( 'NONE',  ( 40.27526882409969744, 125.9297705074273352, 30.44471234641812174 ) ) ;
#4437 = ORIENTED_EDGE ( 'NONE', *, *, #18399, .F. ) ;
#4438 = CARTESIAN_POINT ( 'NONE',  ( 48.01140435219951996, 130.4344580088725820, 32.58608133808903773 ) ) ;
#4439 = VERTEX_POINT ( 'NONE', #9449 ) ;
#4440 = CARTESIAN_POINT ( 'NONE',  ( 43.01140435219951286, 125.6297705074273381, 29.55568802177586463 ) ) ;
#4441 = AXIS2_PLACEMENT_3D ( 'NONE', #15688, #19009, #7766 ) ;
#4442 = CARTESIAN_POINT ( 'NONE',  ( 38.01140435219952707, 72.71049967264873715, 34.21067981925357060 ) ) ;
#4443 = CARTESIAN_POINT ( 'NONE',  ( 43.01140435219951286, 59.03445800887256922, 28.95336869806222779 ) ) ;
#4444 = VECTOR ( 'NONE', #17844, 1000.000000000000000 ) ;
#4445 = CARTESIAN_POINT ( 'NONE',  ( -142.0420953463936087, -195.3938272943107393, 49.65701158161630957 ) ) ;
#4446 = DIRECTION ( 'NONE',  ( -1.140132994654635861E-16, -0.000000000000000000, -1.000000000000000000 ) ) ;
#4447 = CARTESIAN_POINT ( 'NONE',  ( -46.09493621325655255, 160.7104996726487514, -35.00000000000000000 ) ) ;
#4448 = CARTESIAN_POINT ( 'NONE',  ( -161.4692556286852607, -188.6391397928654783, 46.40781461928724383 ) ) ;
#4449 = CARTESIAN_POINT ( 'NONE',  ( 42.21948215057684450, 67.38361825032845331, 39.21067981925355639 ) ) ;
#4450 = CARTESIAN_POINT ( 'NONE',  ( 44.55648932407425633, 93.68445800887258201, 38.96596240072933170 ) ) ;
#4451 = CARTESIAN_POINT ( 'NONE',  ( -142.0420953463936087, -189.3938272943107393, 49.65701158161630957 ) ) ;
#4452 = CARTESIAN_POINT ( 'NONE',  ( 43.01140435219951286, 128.0344580088725763, 28.95336869806222779 ) ) ;
#4453 = CARTESIAN_POINT ( 'NONE',  ( 43.01140435219951286, 104.6297705074273239, 29.55568802177586463 ) ) ;
#4454 = CARTESIAN_POINT ( 'NONE',  ( 71.27174135432656499, 120.9783100490299574, 11.62814500561148456 ) ) ;
#4455 = CARTESIAN_POINT ( 'NONE',  ( -157.2955611005346270, -185.3438272943106995, 41.63779006702063867 ) ) ;
#4456 = CARTESIAN_POINT ( 'NONE',  ( 40.27526882409969744, 96.56518717409400665, 37.97664729208901235 ) ) ;
#4457 = CARTESIAN_POINT ( 'NONE',  ( 147.8787791192428074, -126.9891397928655010, 49.65701158161629536 ) ) ;
#4458 = ORIENTED_EDGE ( 'NONE', *, *, #17049, .F. ) ;
#4459 = CYLINDRICAL_SURFACE ( 'NONE', #21049, 4.999999999999997335 ) ;
#4460 = CARTESIAN_POINT ( 'NONE',  ( 76.04618105687035268, 128.8835079444423286, -1.708432735116285350 ) ) ;
#4461 = VECTOR ( 'NONE', #11444, 1000.000000000000000 ) ;
#4462 = CARTESIAN_POINT ( 'NONE',  ( 66.54750331441660194, 135.2948500229566093, -7.982215242636039321 ) ) ;
#4463 = EDGE_CURVE ( 'NONE', #10265, #14309, #19983, .T. ) ;
#4464 = CARTESIAN_POINT ( 'NONE',  ( 38.58424406990785371, 63.52977050742730825, 35.64915139335015937 ) ) ;
#4465 = ORIENTED_EDGE ( 'NONE', *, *, #12868, .T. ) ;
#4466 = VERTEX_POINT ( 'NONE', #11295 ) ;
#4467 = CARTESIAN_POINT ( 'NONE',  ( 43.01140435219951286, 151.1297705074273097, 38.86567161673127657 ) ) ;
#4468 = CARTESIAN_POINT ( 'NONE',  ( -161.4692556286853176, -193.5630981290892976, 49.65701158161630957 ) ) ;
#4469 = VECTOR ( 'NONE', #6800, 1000.000000000000000 ) ;
#4470 = CARTESIAN_POINT ( 'NONE',  ( 41.46631938032478359, 117.1104996726487428, 29.45539723777780239 ) ) ;
#4472 = CARTESIAN_POINT ( 'NONE',  ( 26.87026879109711786, 150.0197496251087728, 11.30891725959585159 ) ) ;
#4471 = CARTESIAN_POINT ( 'NONE',  ( 38.58424406990786082, 69.11518717409400381, 34.21067981925357060 ) ) ;
#4473 = CARTESIAN_POINT ( 'NONE',  ( 43.01140435219951286, 121.4604996726487371, 39.21067981925356349 ) ) ;
#4474 = CARTESIAN_POINT ( 'NONE',  ( -157.2955611005345986, -175.4438272943107506, 57.67623309621197336 ) ) ;
#4475 = VECTOR ( 'NONE', #16939, 1000.000000000000000 ) ;
#4476 = CARTESIAN_POINT ( 'NONE',  ( 38.01140435219952707, 155.7844580088725763, 34.21067981925357060 ) ) ;
#4477 = CARTESIAN_POINT ( 'NONE',  ( -141.4692556286852891, -183.0630981290892976, 49.65701158161630957 ) ) ;
#4478 = DIRECTION ( 'NONE',  ( 0.000000000000000000, 0.000000000000000000, 1.000000000000000000 ) ) ;
#4479 = CARTESIAN_POINT ( 'NONE',  ( 39.92123440845005433, 150.2344580088725650, 38.46393386101375711 ) ) ;
#4480 = CARTESIAN_POINT ( 'NONE',  ( 38.58424406990786082, 132.3797705074273381, 34.21067981925357060 ) ) ;
#4481 = CARTESIAN_POINT ( 'NONE',  ( 40.94072057685551869, 85.65469043817564909, -0.5939954219232065347 ) ) ;
#4482 = CARTESIAN_POINT ( 'NONE',  ( 47.43856463449118621, 127.6151871740940038, 34.21067981925357060 ) ) ;
#4483 = CARTESIAN_POINT ( 'NONE',  ( 43.01140435219951286, 70.46049967264873715, 39.21067981925356349 ) ) ;
#4484 = CARTESIAN_POINT ( 'NONE',  ( -145.6429501568359797, -159.2084106276439854, 41.63779006702063867 ) ) ;
#4485 = ADVANCED_FACE ( 'NONE', ( #6342 ), #21341, .T. ) ;
#4486 = DIRECTION ( 'NONE',  ( 0.5010362705417046314, -0.000000000000000000, -0.8654262854811262118 ) ) ;
#4487 = FACE_OUTER_BOUND ( 'NONE', #2018, .T. ) ;
#4488 = ADVANCED_FACE ( 'NONE', ( #12959 ), #2928, .F. ) ;
#4489 = CARTESIAN_POINT ( 'NONE',  ( 66.79315400704923888, 104.7533658121278819, -7.700889860664787534 ) ) ;
#4490 = VECTOR ( 'NONE', #1299, 1000.000000000000000 ) ;
#4491 = CYLINDRICAL_SURFACE ( 'NONE', #20957, 27.58651506682278765 ) ;
#4492 = CARTESIAN_POINT ( 'NONE',  ( 44.37947211624943833, 104.2151871740939981, 30.00020018409699318 ) ) ;
#4493 = ORIENTED_EDGE ( 'NONE', *, *, #11250, .T. ) ;
#4494 = EDGE_CURVE ( 'NONE', #1056, #14631, #20223, .T. ) ;
#4495 = DIRECTION ( 'NONE',  ( 1.723963091245776585E-16, 6.336983651701954299E-17, 1.000000000000000000 ) ) ;
#4496 = ORIENTED_EDGE ( 'NONE', *, *, #6638, .T. ) ;
#4497 = CARTESIAN_POINT ( 'NONE',  ( 47.05648932407426344, 84.98445800887257917, 37.14960608071593384 ) ) ;
#4498 = DIRECTION ( 'NONE',  ( 0.000000000000000000, -1.000000000000000000, 0.000000000000000000 ) ) ;
#4499 = CARTESIAN_POINT ( 'NONE',  ( 41.46631938032478359, 147.1104996726487570, 29.45539723777780239 ) ) ;
#4501 = CARTESIAN_POINT ( 'NONE',  ( 63.64508858465791974, 100.8029030738736225, 7.494358438614500351 ) ) ;
#4500 = CARTESIAN_POINT ( 'NONE',  ( 47.43856463449117200, 103.7651871740939669, 32.77220824515698183 ) ) ;
#4502 = CARTESIAN_POINT ( 'NONE',  ( -143.8425227516148084, -171.3584106276440764, 44.11586579668791330 ) ) ;
#4503 = CARTESIAN_POINT ( 'NONE',  ( 46.10157429594899270, 61.76049967264873430, 38.46393386101376421 ) ) ;
#4505 = FACE_OUTER_BOUND ( 'NONE', #6908, .T. ) ;
#4504 = CARTESIAN_POINT ( 'NONE',  ( 44.31473939091409875, 144.8751687964759469, 39.04902473919937478 ) ) ;
#4506 = CARTESIAN_POINT ( 'NONE',  ( 43.01140435219951286, 117.5344580088725763, 39.21067981925356349 ) ) ;
#4507 = EDGE_CURVE ( 'NONE', #3649, #19172, #20029, .T. ) ;
#4508 = DIRECTION ( 'NONE',  ( -1.000000000000000000, 0.000000000000000000, 0.000000000000000000 ) ) ;
#4509 = LINE ( 'NONE', #7514, #7635 ) ;
#4510 = CARTESIAN_POINT ( 'NONE',  ( 46.59305225739526435, 64.31518717409399244, 36.81289934271958941 ) ) ;
#4511 = CARTESIAN_POINT ( 'NONE',  ( 75.85495621331871519, 129.5603373922052697, -8.732165470513974626 ) ) ;
#4512 = CARTESIAN_POINT ( 'NONE',  ( 47.43856463449118621, 151.6151871740939896, 34.21067981925357060 ) ) ;
#4513 = DIRECTION ( 'NONE',  ( 0.000000000000000000, -1.000000000000000000, 0.000000000000000000 ) ) ;
#4514 = CARTESIAN_POINT ( 'NONE',  ( -160.8964159109769696, -172.8938272943107393, 49.65701158161630957 ) ) ;
#4515 = CARTESIAN_POINT ( 'NONE',  ( -151.4692556286852891, -188.9084106276440593, 39.74470866294723947 ) ) ;
#4516 = EDGE_CURVE ( 'NONE', #14601, #19802, #20478, .T. ) ;
#4517 = ORIENTED_EDGE ( 'NONE', *, *, #10557, .T. ) ;
#4518 = CARTESIAN_POINT ( 'NONE',  ( 39.42975644700377558, 72.41518717409400097, 36.81289934271958941 ) ) ;
#4519 = CARTESIAN_POINT ( 'NONE',  ( -145.6429501568359797, -166.1084106276440480, 57.67623309621198047 ) ) ;
#4520 = CARTESIAN_POINT ( 'NONE',  ( 76.43728072391715500, 127.6653364257898744, 18.33484128816649772 ) ) ;
#4521 = CARTESIAN_POINT ( 'NONE',  ( 43.01140435219951286, 111.5344580088725905, 39.21067981925356349 ) ) ;
#4522 = CARTESIAN_POINT ( 'NONE',  ( 40.27526882409969033, 131.6651871740939725, 30.44471234641811819 ) ) ;
#4523 = CARTESIAN_POINT ( 'NONE',  ( 54.72474920843421131, 151.9887481548900325, -8.775581469602226292 ) ) ;
#4524 = EDGE_LOOP ( 'NONE', ( #21426, #12231, #11115, #17402 ) ) ;
#4525 = VERTEX_POINT ( 'NONE', #2041 ) ;
#4526 = ADVANCED_BREP_SHAPE_REPRESENTATION ( '', ( #62, #12657 ), #2455 ) ;
#4527 =( NAMED_UNIT ( * ) PLANE_ANGLE_UNIT ( ) SI_UNIT ( $, .RADIAN. ) );
#4528 = ORIENTED_EDGE ( 'NONE', *, *, #16312, .T. ) ;
#4529 = CARTESIAN_POINT ( 'NONE',  ( 48.01140435219951996, 109.1344580088725849, 35.83527830041810347 ) ) ;
#4530 = DIRECTION ( 'NONE',  ( 0.4938165983075534227, -0.8695660798558993987, 0.000000000000000000 ) ) ;
#4531 = CARTESIAN_POINT ( 'NONE',  ( 40.27526882409969033, 77.92977050742732104, 30.44471234641811819 ) ) ;
#4532 = CARTESIAN_POINT ( 'NONE',  ( 38.58424406990784661, 134.9651871740940123, 32.77220824515698183 ) ) ;
#4533 = CARTESIAN_POINT ( 'NONE',  ( 39.92123440845004723, 87.26049967264874851, 29.95742577749337343 ) ) ;
#4534 = CARTESIAN_POINT ( 'NONE',  ( 8.798315742295939046, 121.0924013121165075, 9.124689178586496752 ) ) ;
#4535 = CARTESIAN_POINT ( 'NONE',  ( 42.35941266477436784, 94.91347937787368494, 29.24238570022250983 ) ) ;
#4536 = CARTESIAN_POINT ( 'NONE',  ( -148.3790856849358306, -163.5891397928654669, 59.16757674456786020 ) ) ;
#4537 = CARTESIAN_POINT ( 'NONE',  ( 40.27526882409969033, 83.66518717409398675, 30.44471234641811819 ) ) ;
#4538 = CARTESIAN_POINT ( 'NONE',  ( 48.01140435219951996, 107.3604996726487428, 32.58608133808903773 ) ) ;
#4539 = CYLINDRICAL_SURFACE ( 'NONE', #13184, 10.00000000000000888 ) ;
#4540 = CARTESIAN_POINT ( 'NONE',  ( 44.55648932407425633, 61.61049967264874283, 38.96596240072933170 ) ) ;
#4541 = ORIENTED_EDGE ( 'NONE', *, *, #9639, .F. ) ;
#4542 = CARTESIAN_POINT ( 'NONE',  ( 47.43856463449117200, 76.72977050742733240, 35.64915139335016647 ) ) ;
#4543 = CARTESIAN_POINT ( 'NONE',  ( -142.0420953463936087, -159.3938272943107393, 49.65701158161630957 ) ) ;
#4544 = CARTESIAN_POINT ( 'NONE',  ( 42.92180000979148957, 85.67454126555050209, 7.339147150375312734 ) ) ;
#4545 = VECTOR ( 'NONE', #21609, 1000.000000000000000 ) ;
#4546 = CARTESIAN_POINT ( 'NONE',  ( -142.0420953463936087, -186.6584106276440309, 49.65701158161630957 ) ) ;
#4547 = ORIENTED_EDGE ( 'NONE', *, *, #3159, .T. ) ;
#4548 = FACE_OUTER_BOUND ( 'NONE', #6072, .T. ) ;
#4549 = AXIS2_PLACEMENT_3D ( 'NONE', #1856, #11988, #3730 ) ;
#4550 = CARTESIAN_POINT ( 'NONE',  ( 38.96631938032478359, 105.0844580088725877, 37.14960608071593384 ) ) ;
#4551 = CARTESIAN_POINT ( 'NONE',  ( 41.64333658814960870, 128.7797705074273438, 30.00020018409699318 ) ) ;
#4552 = VERTEX_POINT ( 'NONE', #10211 ) ;
#4553 = CYLINDRICAL_SURFACE ( 'NONE', #18890, 4.999999999999997335 ) ;
#4554 = ORIENTED_EDGE ( 'NONE', *, *, #18688, .T. ) ;
#4555 = CARTESIAN_POINT ( 'NONE',  ( 45.74753988029933538, 128.3297705074273267, 30.44471234641811819 ) ) ;
#4556 = FACE_OUTER_BOUND ( 'NONE', #10267, .T. ) ;
#4557 = CARTESIAN_POINT ( 'NONE',  ( 39.92123440845004723, 66.23445800887257917, 38.46393386101376421 ) ) ;
#4558 =( BOUNDED_CURVE ( )  B_SPLINE_CURVE ( 2, ( #15595, #502, #20678, #7346, #9108, #5562, #14050, #5674, #14157, #8996, #20783, #15807, #721 ),
 .UNSPECIFIED., .F., .F. ) 
 B_SPLINE_CURVE_WITH_KNOTS ( ( 3, 2, 2, 2, 2, 2, 3 ),
 ( 0.3602941176470588203, 0.3617647058823529327, 0.3647058823529411575, 0.3676470588235294379, 0.3705882352941176627, 0.3735294117647058876, 0.3750000000000000000 ),
 .UNSPECIFIED. ) 
 CURVE ( )  GEOMETRIC_REPRESENTATION_ITEM ( )  RATIONAL_B_SPLINE_CURVE ( ( 0.9755282581475768211, 0.9755282581475768211, 1.000000000000000000, 0.9510565162951535312, 1.000000000000000000, 0.9510565162951535312, 1.000000000000000000, 0.9510565162951535312, 1.000000000000000000, 0.9510565162951535312, 1.000000000000000000, 0.9755282581475768211, 0.9755282581475768211 ) ) 
 REPRESENTATION_ITEM ( '' )  );
#4559 = EDGE_CURVE ( 'NONE', #2742, #10861, #10424, .T. ) ;
#4560 = VECTOR ( 'NONE', #5254, 1000.000000000000000 ) ;
#4561 = DIRECTION ( 'NONE',  ( 1.000000000000000000, 0.000000000000000000, 0.000000000000000000 ) ) ;
#4562 = DIRECTION ( 'NONE',  ( -0.000000000000000000, -0.000000000000000000, -1.000000000000000000 ) ) ;
#4563 = CARTESIAN_POINT ( 'NONE',  ( -157.6495955161842062, -191.9391397928654612, 41.15050349809590102 ) ) ;
#4564 = CARTESIAN_POINT ( 'NONE',  ( 38.96631938032478359, 156.4104996726487400, 31.27175355779120025 ) ) ;
#4565 = CARTESIAN_POINT ( 'NONE',  ( 43.01140435219951286, 103.4604996726487371, 39.21067981925356349 ) ) ;
#4566 = CARTESIAN_POINT ( 'NONE',  ( -159.0959885057557983, -193.5938272943107279, 55.19815736654470584 ) ) ;
#4567 = CARTESIAN_POINT ( 'NONE',  ( 48.01140435219951996, 121.4344580088725820, 32.58608133808903773 ) ) ;
#4568 = CARTESIAN_POINT ( 'NONE',  ( 40.27526882409969033, 108.8297705074272983, 37.97664729208901946 ) ) ;
#4569 = CARTESIAN_POINT ( 'NONE',  ( 41.61464536962099459, 148.1530905165343768, 16.86614982034995691 ) ) ;
#4570 = CARTESIAN_POINT ( 'NONE',  ( -154.3824083646099439, -185.4938272943107336, 40.69124936498395328 ) ) ;
#4571 = CARTESIAN_POINT ( 'NONE',  ( 46.59305225739526435, 100.3151871740940067, 36.81289934271958941 ) ) ;
#4572 = CYLINDRICAL_SURFACE ( 'NONE', #15764, 4.999999999999997335 ) ;
#4573 = VERTEX_POINT ( 'NONE', #6573 ) ;
#4574 = CARTESIAN_POINT ( 'NONE',  ( 159.6377923430271153, 201.9209935688625421, 21.73429951086134082 ) ) ;
#4575 = CARTESIAN_POINT ( 'NONE',  ( 75.80354157443048280, 110.0810758630161672, 5.910575721798123183 ) ) ;
#4576 = CARTESIAN_POINT ( 'NONE',  ( 35.06472793454997117, 92.93335285089702325, -12.26792952838020767 ) ) ;
#4577 = EDGE_CURVE ( 'NONE', #17533, #10563, #8559, .T. ) ;
#4578 = CARTESIAN_POINT ( 'NONE',  ( 47.43856463449118621, 70.87977050742732388, 34.21067981925357060 ) ) ;
#4579 = ORIENTED_EDGE ( 'NONE', *, *, #490, .T. ) ;
#4580 = ORIENTED_EDGE ( 'NONE', *, *, #19729, .T. ) ;
#4581 = CARTESIAN_POINT ( 'NONE',  ( 43.01140435219951286, 154.1297705074273097, 38.86567161673127657 ) ) ;
#4582 = LINE ( 'NONE', #6463, #12990 ) ;
#4583 = CARTESIAN_POINT ( 'NONE',  ( 38.01140435219951996, 111.5604996726487599, 32.58608133808903773 ) ) ;
#4584 = CARTESIAN_POINT ( 'NONE',  ( 46.59305225739526435, 70.91518717409398675, 31.60846029578754468 ) ) ;
#4585 = FACE_BOUND ( 'NONE', #17508, .T. ) ;
#4586 = CARTESIAN_POINT ( 'NONE',  ( -160.8964159109769696, -160.8938272943107393, 49.65701158161630957 ) ) ;
#4587 = CARTESIAN_POINT ( 'NONE',  ( -149.8854112254399240, -166.6622583705451746, 59.65701158161632378 ) ) ;
#4588 = CARTESIAN_POINT ( 'NONE',  ( -159.5594255724347761, -175.8630981290893089, 43.77915905869157598 ) ) ;
#4589 =( NAMED_UNIT ( * ) PLANE_ANGLE_UNIT ( ) SI_UNIT ( $, .RADIAN. ) );
#4590 = PRESENTATION_LAYER_ASSIGNMENT (  '', '', ( #14803 ) ) ;
#4591 = DIRECTION ( 'NONE',  ( -1.000000000000000000, 0.000000000000000000, 0.000000000000000000 ) ) ;
#4593 = ADVANCED_FACE ( 'NONE', ( #3373, #3261 ), #10097, .F. ) ;
#4592 = CARTESIAN_POINT ( 'NONE',  ( 38.96631938032478359, 156.0844580088725877, 37.14960608071593384 ) ) ;
#4594 = CARTESIAN_POINT ( 'NONE',  ( 46.59305225739526435, 134.1797705074273210, 31.60846029578754468 ) ) ;
#4595 = CARTESIAN_POINT ( 'NONE',  ( 10.76517401744387215, 131.6399553617083029, 15.47769843104460463 ) ) ;
#4596 = CARTESIAN_POINT ( 'NONE',  ( 38.58424406990785371, 128.9651871740940123, 32.77220824515697473 ) ) ;
#4597 = CARTESIAN_POINT ( 'NONE',  ( 145.5008360144876747, 198.5836349573982886, 34.00000000000001421 ) ) ;
#4598 = CARTESIAN_POINT ( 'NONE',  ( -143.8425227516148084, -159.3584106276440480, 44.11586579668791330 ) ) ;
#4599 = CARTESIAN_POINT ( 'NONE',  ( 48.01140435219951996, 140.2104996726487514, 34.21067981925357060 ) ) ;
#4600 = FACE_OUTER_BOUND ( 'NONE', #20484, .T. ) ;
#4601 = CARTESIAN_POINT ( 'NONE',  ( 15.06790588970514833, 124.2609462974868677, 22.34264618625151044 ) ) ;
#4602 = LINE ( 'NONE', #2737, #736 ) ;
#4603 = VERTEX_POINT ( 'NONE', #1928 ) ;
#4604 = ADVANCED_FACE ( 'NONE', ( #9992 ), #1603, .T. ) ;
#4605 = CARTESIAN_POINT ( 'NONE',  ( 147.8787791192428074, -126.9891397928655010, 10.34298841838370642 ) ) ;
#4606 = ORIENTED_EDGE ( 'NONE', *, *, #333, .F. ) ;
#4607 = CARTESIAN_POINT ( 'NONE',  ( 48.01140435219951996, 79.43445800887258201, 32.58608133808903773 ) ) ;
#4608 = FACE_OUTER_BOUND ( 'NONE', #15828, .T. ) ;
#4609 = CARTESIAN_POINT ( 'NONE',  ( 48.01140435219951996, 143.0604996726487173, 35.83527830041810347 ) ) ;
#4611 = CARTESIAN_POINT ( 'NONE',  ( 19.79626631456835284, 104.0394230781280669, 2.494070082984220171 ) ) ;
#4610 = CARTESIAN_POINT ( 'NONE',  ( 38.58424406990786082, 99.11518717409400381, 34.21067981925357060 ) ) ;
#4612 = EDGE_CURVE ( 'NONE', #18469, #10856, #58, .T. ) ;
#4613 = CARTESIAN_POINT ( 'NONE',  ( -159.0959885057557983, -166.8584106276440480, 55.19815736654470584 ) ) ;
#4614 = CARTESIAN_POINT ( 'NONE',  ( 48.01140435219951996, 62.06049967264872436, 35.83527830041810347 ) ) ;
#4616 = DIRECTION ( 'NONE',  ( -0.000000000000000000, 0.000000000000000000, 1.000000000000000000 ) ) ;
#4615 = CARTESIAN_POINT ( 'NONE',  ( -151.4692556286852607, -165.8130981290893260, 59.65701158161632378 ) ) ;
#4617 = CARTESIAN_POINT ( 'NONE',  ( 54.85617982533816672, 239.2521282348021714, -19.99999999999996092 ) ) ;
#4618 = FACE_OUTER_BOUND ( 'NONE', #16919, .T. ) ;
#4619 = CARTESIAN_POINT ( 'NONE',  ( 42.21948215057684450, 79.38361825032846752, 39.21067981925355639 ) ) ;
#4620 =( BOUNDED_CURVE ( )  B_SPLINE_CURVE ( 2, ( #8159, #11782, #20279, #11447, #20177, #3194, #18405, #8052, #1650, #5173, #8271, #15090, #18061 ),
 .UNSPECIFIED., .F., .F. ) 
 B_SPLINE_CURVE_WITH_KNOTS ( ( 3, 2, 2, 2, 2, 2, 3 ),
 ( 0.4107142857142857539, 0.4142857142857143127, 0.4214285714285714302, 0.4285714285714285476, 0.4357142857142857206, 0.4428571428571428381, 0.4464285714285714524 ),
 .UNSPECIFIED. ) 
 CURVE ( )  GEOMETRIC_REPRESENTATION_ITEM ( )  RATIONAL_B_SPLINE_CURVE ( ( 0.9755282581475768211, 0.9755282581475769321, 1.000000000000000000, 0.9510565162951535312, 1.000000000000000000, 0.9510565162951535312, 1.000000000000000000, 0.9510565162951535312, 1.000000000000000000, 0.9510565162951535312, 1.000000000000000000, 0.9755282581475765991, 0.9755282581475768211 ) ) 
 REPRESENTATION_ITEM ( '' )  );
#4621 = CARTESIAN_POINT ( 'NONE',  ( 39.42975644700377558, 159.0797705074273267, 31.60846029578754468 ) ) ;
#4622 = CARTESIAN_POINT ( 'NONE',  ( 77.22939692449374149, 120.9137088693742044, 5.553548964694690504 ) ) ;
#4623 = CARTESIAN_POINT ( 'NONE',  ( 39.42975644700377558, 153.4151871740940010, 36.81289934271958941 ) ) ;
#4624 = PLANE ( 'NONE',  #20503 ) ;
#4625 = CARTESIAN_POINT ( 'NONE',  ( -142.0420953463936087, -168.3938272943107393, 49.65701158161630957 ) ) ;
#4626 = CARTESIAN_POINT ( 'NONE',  ( -160.8964159109769696, -188.0084106276440252, 52.72008163687743121 ) ) ;
#4627 = ORIENTED_EDGE ( 'NONE', *, *, #11087, .T. ) ;
#4628 = CARTESIAN_POINT ( 'NONE',  ( 47.43856463449118621, 67.61518717409398960, 34.21067981925357060 ) ) ;
#4629 = CARTESIAN_POINT ( 'NONE',  ( -160.8964159109769696, -173.0084106276440821, 52.72008163687743121 ) ) ;
#4630 = CARTESIAN_POINT ( 'NONE',  ( 11.40453246296876877, 106.5480838228176452, 14.64419766361223552 ) ) ;
#4631 = DIRECTION ( 'NONE',  ( 0.000000000000000000, 1.000000000000000000, 0.000000000000000000 ) ) ;
#4632 = CARTESIAN_POINT ( 'NONE',  ( 45.74753988029933538, 130.1651871740940010, 37.97664729208901946 ) ) ;
#4633 = CARTESIAN_POINT ( 'NONE',  ( 74.70172802024292480, 107.1710682803345662, -6.989838304517381751 ) ) ;
#4634 = ORIENTED_EDGE ( 'NONE', *, *, #10310, .T. ) ;
#4635 = ORIENTED_EDGE ( 'NONE', *, *, #3566, .T. ) ;
#4636 = AXIS2_PLACEMENT_3D ( 'NONE', #12352, #4198, #18976 ) ;
#4637 = EDGE_CURVE ( 'NONE', #9746, #9069, #4827, .T. ) ;
#4638 = AXIS2_PLACEMENT_3D ( 'NONE', #18358, #13178, #19910 ) ;
#4639 = CARTESIAN_POINT ( 'NONE',  ( 53.64127281404707048, 146.0262708631457542, 11.34682183016344403 ) ) ;
#4640 = ORIENTED_EDGE ( 'NONE', *, *, #21212, .T. ) ;
#4641 = CARTESIAN_POINT ( 'NONE',  ( 41.46631938032478359, 110.1844580088725820, 29.45539723777780239 ) ) ;
#4642 = DIRECTION ( 'NONE',  ( 1.000000000000000000, 0.000000000000000000, 0.000000000000000000 ) ) ;
#4643 = AXIS2_PLACEMENT_3D ( 'NONE', #13010, #19731, #5950 ) ;
#4644 = CARTESIAN_POINT ( 'NONE',  ( 47.43856463449118621, 76.87977050742732388, 34.21067981925357060 ) ) ;
#4646 = CARTESIAN_POINT ( 'NONE',  ( 34.07414013685151843, 93.16113583794900421, 7.775673839875955728 ) ) ;
#4645 = CARTESIAN_POINT ( 'NONE',  ( 45.74753988029933538, 125.0651871740940209, 30.44471234641811819 ) ) ;
#4647 = CARTESIAN_POINT ( 'NONE',  ( 41.46631938032478359, 93.11049967264874283, 29.45539723777780239 ) ) ;
#4648 = LINE ( 'NONE', #11367, #4085 ) ;
#4649 = CARTESIAN_POINT ( 'NONE',  ( 39.70842430446096216, 95.12513732185091442, 30.44285285587857004 ) ) ;
#4650 = CARTESIAN_POINT ( 'NONE',  ( -141.4692556286852891, -163.1391397928655067, 52.90620854394536821 ) ) ;
#4651 = CARTESIAN_POINT ( 'NONE',  ( 41.64333658814960870, 89.51518717409399528, 30.00020018409699318 ) ) ;
#4652 = PRODUCT_DEFINITION_CONTEXT ( 'detailed design', #18727, 'design' ) ;
#4653 = CARTESIAN_POINT ( 'NONE',  ( 96.62434152388763664, 220.7958015105191976, 4.000000000000021316 ) ) ;
#4654 = CARTESIAN_POINT ( 'NONE',  ( 48.01140435219951996, 71.21049967264873715, 34.21067981925357060 ) ) ;
#4655 = PRODUCT_DEFINITION_SHAPE ( 'NONE', 'NONE',  #21825 ) ;
#4656 =( GEOMETRIC_REPRESENTATION_CONTEXT ( 3 ) GLOBAL_UNCERTAINTY_ASSIGNED_CONTEXT ( ( #17219 ) ) GLOBAL_UNIT_ASSIGNED_CONTEXT ( ( #19634, #4527, #9617 ) ) REPRESENTATION_CONTEXT ( 'NONE', 'WORKASPACE' ) );
#4657 = FACE_OUTER_BOUND ( 'NONE', #17184, .T. ) ;
#4658 = EDGE_LOOP ( 'NONE', ( #12688, #8306, #8008, #21182 ) ) ;
#4659 = CARTESIAN_POINT ( 'NONE',  ( 39.42975644700377558, 75.67977050742732104, 36.81289934271958941 ) ) ;
#4660 = CARTESIAN_POINT ( 'NONE',  ( -142.0420953463936087, -192.6584106276440593, 49.65701158161630957 ) ) ;
#4661 = CARTESIAN_POINT ( 'NONE',  ( 21.43032318156618388, 146.4805633285969861, 10.07716523980869816 ) ) ;
#4662 = CARTESIAN_POINT ( 'NONE',  ( -159.0959885057557983, -181.8584106276440480, 55.19815736654470584 ) ) ;
#4663 = ORIENTED_EDGE ( 'NONE', *, *, #15541, .T. ) ;
#4664 = DIRECTION ( 'NONE',  ( -1.000000000000000000, 0.000000000000000000, 0.000000000000000000 ) ) ;
#4665 = CARTESIAN_POINT ( 'NONE',  ( 93.25569916848381524, 126.0916958004080755, -19.99999999999997868 ) ) ;
#4666 = CARTESIAN_POINT ( 'NONE',  ( 43.01140435219951286, 121.1297705074273097, 38.86567161673127657 ) ) ;
#4667 = ORIENTED_EDGE ( 'NONE', *, *, #7095, .F. ) ;
#4668 = ADVANCED_FACE ( 'NONE', ( #13609 ), #20347, .F. ) ;
#4669 = ORIENTED_EDGE ( 'NONE', *, *, #7673, .F. ) ;
#4670 = CYLINDRICAL_SURFACE ( 'NONE', #231, 10.00000000000000888 ) ;
#4671 = CARTESIAN_POINT ( 'NONE',  ( 38.01140435219951996, 62.63445800887255643, 32.58608133808903773 ) ) ;
#4672 = CARTESIAN_POINT ( 'NONE',  ( 43.01140435219951286, 143.9604996726487229, 29.21067981925356705 ) ) ;
#4673 = CARTESIAN_POINT ( 'NONE',  ( 138.2733499813809885, 177.2661675079481540, -44.99999999999997158 ) ) ;
#4674 = CARTESIAN_POINT ( 'NONE',  ( -47.86331837773882825, -37.13255853780189852, -35.00000000000000000 ) ) ;
#4675 = CARTESIAN_POINT ( 'NONE',  ( -145.2889157411863721, -190.4391397928654612, 58.16351966513671812 ) ) ;
#4676 = CARTESIAN_POINT ( 'NONE',  ( -176.9699209214867608, -126.9891397928655010, 67.64809332337415526 ) ) ;
#4677 = CARTESIAN_POINT ( 'NONE',  ( 43.01140435219951286, 101.9604996726487371, 29.21067981925356705 ) ) ;
#4678 = CARTESIAN_POINT ( 'NONE',  ( -159.0959885057557983, -191.1938272943107222, 44.11586579668791330 ) ) ;
#4679 = SHAPE_DEFINITION_REPRESENTATION ( #16619, #5457 ) ;
#4680 = CARTESIAN_POINT ( 'NONE',  ( 38.96631938032478359, 120.0844580088725735, 37.14960608071593384 ) ) ;
#4681 = CARTESIAN_POINT ( 'NONE',  ( 39.42975644700377558, 108.0797705074273125, 31.60846029578754468 ) ) ;
#4682 = CARTESIAN_POINT ( 'NONE',  ( 15.94687047784549172, 111.7036002239776451, 14.84254118869207417 ) ) ;
#4683 = CARTESIAN_POINT ( 'NONE',  ( -143.8425227516148084, -180.0938272943107279, 44.11586579668791330 ) ) ;
#4684 = CARTESIAN_POINT ( 'NONE',  ( 46.59305225739526435, 85.91518717409400097, 31.60846029578754468 ) ) ;
#4685 = LINE ( 'NONE', #11401, #6629 ) ;
#4686 = ORIENTED_EDGE ( 'NONE', *, *, #10967, .T. ) ;
#4687 = CARTESIAN_POINT ( 'NONE',  ( 68.29446192123552350, 96.82662215664792882, 13.41040346623746515 ) ) ;
#4688 = CARTESIAN_POINT ( 'NONE',  ( 17.40773937504753377, 131.5336607133424991, -10.36307277412196903 ) ) ;
#4689 = EDGE_CURVE ( 'NONE', #20856, #7746, #10501, .T. ) ;
#4690 = CARTESIAN_POINT ( 'NONE',  ( 40.27526882409969744, 62.92977050742730682, 30.44471234641812174 ) ) ;
#4691 = VERTEX_POINT ( 'NONE', #2146 ) ;
#4692 = ORIENTED_EDGE ( 'NONE', *, *, #4769, .T. ) ;
#4693 = CARTESIAN_POINT ( 'NONE',  ( 44.37947211624943833, 143.4797705074273324, 30.00020018409699318 ) ) ;
#4694 = CARTESIAN_POINT ( 'NONE',  ( -151.4692556286852891, -189.8130981290892976, 59.65701158161632378 ) ) ;
#4695 = CARTESIAN_POINT ( 'NONE',  ( 48.01140435219951996, 113.3604996726487286, 32.58608133808903773 ) ) ;
#4696 = CARTESIAN_POINT ( 'NONE',  ( 47.43856463449118621, 64.61518717409398960, 34.21067981925357060 ) ) ;
#4697 = DIRECTION ( 'NONE',  ( 0.000000000000000000, 0.000000000000000000, -1.000000000000000000 ) ) ;
#4698 = CARTESIAN_POINT ( 'NONE',  ( -160.8964159109769696, -164.0438272943107165, 46.59394152635518083 ) ) ;
#4699 = CARTESIAN_POINT ( 'NONE',  ( 163.3023584364855196, 191.8436256089667324, 20.54250398750395590 ) ) ;
#4700 = CARTESIAN_POINT ( 'NONE',  ( -159.5594255724347761, -175.2630981290893146, 55.53486410454104316 ) ) ;
#4701 = DIRECTION ( 'NONE',  ( -0.000000000000000000, -0.000000000000000000, -1.000000000000000000 ) ) ;
#4702 = CARTESIAN_POINT ( 'NONE',  ( 48.01140435219951996, 148.1344580088725706, 35.83527830041810347 ) ) ;
#4703 = CARTESIAN_POINT ( 'NONE',  ( 44.37947211624943833, 128.4797705074273040, 30.00020018409699318 ) ) ;
#4704 = CARTESIAN_POINT ( 'NONE',  ( 41.39294982251618649, 154.1830292177732531, 16.78735015533800734 ) ) ;
#4705 = CARTESIAN_POINT ( 'NONE',  ( 44.37947211624943833, 113.2151871740940123, 30.00020018409699318 ) ) ;
#4706 = DIRECTION ( 'NONE',  ( -0.000000000000000000, 1.000000000000000000, -0.000000000000000000 ) ) ;
#4707 = AXIS2_PLACEMENT_3D ( 'NONE', #4457, #21235, #10880 ) ;
#4708 = CARTESIAN_POINT ( 'NONE',  ( 43.01140435219951996, 151.4604996726487514, 39.21067981925356349 ) ) ;
#4709 = CARTESIAN_POINT ( 'NONE',  ( 45.51140435220141001, 58.78519719078001060, 29.88055280033245964 ) ) ;
#4710 = CARTESIAN_POINT ( 'NONE',  ( 38.01140435219952707, 135.5604996726487457, 32.58608133808903773 ) ) ;
#4711 = CARTESIAN_POINT ( 'NONE',  ( 51.52566954327383542, 92.93877768781105431, 20.08059929855049219 ) ) ;
#4712 = CARTESIAN_POINT ( 'NONE',  ( 44.55648932407425633, 83.81049967264874567, 29.45539723777780239 ) ) ;
#4713 = ORIENTED_EDGE ( 'NONE', *, *, #19345, .F. ) ;
#4714 = FACE_OUTER_BOUND ( 'NONE', #2113, .T. ) ;
#4715 = EDGE_LOOP ( 'NONE', ( #13255, #818, #19200, #6200 ) ) ;
#4716 = CARTESIAN_POINT ( 'NONE',  ( 41.46631938032478359, 78.38445800887257064, 38.96596240072933170 ) ) ;
#4717 = CARTESIAN_POINT ( 'NONE',  ( 48.01140435219951996, 103.1344580088725706, 35.83527830041809636 ) ) ;
#4718 = CARTESIAN_POINT ( 'NONE',  ( 44.55648932407425633, 143.8104996726487457, 29.45539723777780239 ) ) ;
#4720 = CARTESIAN_POINT ( 'NONE',  ( 25.97839122281734703, 97.53232036182296838, 2.136956866322798021 ) ) ;
#4719 = CARTESIAN_POINT ( 'NONE',  ( 40.27526882409969033, 101.6651871740940152, 30.44471234641811819 ) ) ;
#4721 = DIRECTION ( 'NONE',  ( -0.000000000000000000, -0.000000000000000000, 1.000000000000000000 ) ) ;
#4722 = CARTESIAN_POINT ( 'NONE',  ( -143.8425227516148084, -165.9584106276440423, 55.19815736654470584 ) ) ;
#4723 = CARTESIAN_POINT ( 'NONE',  ( -143.8425227516148084, -192.6938272943107222, 55.19815736654470584 ) ) ;
#4725 = DIRECTION ( 'NONE',  ( -1.723963091245776092E-16, -6.336983651701951834E-17, -1.000000000000000000 ) ) ;
#4724 = FACE_BOUND ( 'NONE', #8639, .T. ) ;
#4726 = CARTESIAN_POINT ( 'NONE',  ( 38.96631938032478359, 105.4104996726487400, 31.27175355779120025 ) ) ;
#4727 = CARTESIAN_POINT ( 'NONE',  ( 43.01140435219951286, 115.4604996726487229, 39.21067981925356349 ) ) ;
#4728 = CARTESIAN_POINT ( 'NONE',  ( 43.01140435219951286, 79.46049967264875136, 39.21067981925356349 ) ) ;
#4729 = EDGE_CURVE ( 'NONE', #19857, #20247, #894, .T. ) ;
#4730 = CARTESIAN_POINT ( 'NONE',  ( 45.74753988029933538, 65.06518717409400665, 30.44471234641811819 ) ) ;
#4731 = CARTESIAN_POINT ( 'NONE',  ( 41.46631938032478359, 63.38445800887257064, 38.96596240072933170 ) ) ;
#4732 = CARTESIAN_POINT ( 'NONE',  ( 29.43094928344231320, 88.48265962617873015, 0.7917390523231137012 ) ) ;
#4733 = CARTESIAN_POINT ( 'NONE',  ( -148.5561028927606344, -159.9938272943107336, 58.62277379824867296 ) ) ;
#4734 = CARTESIAN_POINT ( 'NONE',  ( -157.2955611005345986, -188.6084106276440480, 41.63779006702063867 ) ) ;
#4735 = ORIENTED_EDGE ( 'NONE', *, *, #4151, .T. ) ;
#4736 = CARTESIAN_POINT ( 'NONE',  ( 46.59305225739526435, 70.91518717409398675, 31.60846029578754468 ) ) ;
#4737 = CARTESIAN_POINT ( 'NONE',  ( -157.2955611005346270, -172.7084106276440423, 57.67623309621198047 ) ) ;
#4738 = CARTESIAN_POINT ( 'NONE',  ( 17.22388115030108224, 97.27017246186569821, 14.28717435998666296 ) ) ;
#4739 = DIRECTION ( 'NONE',  ( 1.000000000000000000, 0.000000000000000000, 0.000000000000000000 ) ) ;
#4740 = CARTESIAN_POINT ( 'NONE',  ( 40.27526882409969033, 129.5651871740940067, 37.97664729208901946 ) ) ;
#4741 = CARTESIAN_POINT ( 'NONE',  ( 47.07528247981900904, 85.99676402675389397, -5.799316066731655006 ) ) ;
#4742 = ORIENTED_EDGE ( 'NONE', *, *, #12062, .T. ) ;
#4743 = EDGE_LOOP ( 'NONE', ( #19322, #8584, #17876, #20034 ) ) ;
#4744 = CARTESIAN_POINT ( 'NONE',  ( 69.68673170630326297, 129.0522134326295145, 12.29911014595921692 ) ) ;
#4745 = VERTEX_POINT ( 'NONE', #7338 ) ;
#4746 = CARTESIAN_POINT ( 'NONE',  ( 43.01140435219951286, 108.5344580088725763, 39.46799094044489209 ) ) ;
#4747 = DIRECTION ( 'NONE',  ( 0.000000000000000000, 0.000000000000000000, 1.000000000000000000 ) ) ;
#4748 = CARTESIAN_POINT ( 'NONE',  ( 39.42975644700377558, 69.67977050742732104, 36.81289934271958941 ) ) ;
#4750 = CARTESIAN_POINT ( 'NONE',  ( 22.56676867748217674, 139.3294883087844198, 3.013676707730225779 ) ) ;
#4749 = CARTESIAN_POINT ( 'NONE',  ( 38.58424406990784661, 129.2651871740940237, 35.64915139335016647 ) ) ;
#4751 =( BOUNDED_CURVE ( )  B_SPLINE_CURVE ( 2, ( #20343, #7114, #8876, #5341, #3172, #13819, #1925, #11955, #4819, #15382, #6899, #18894, #5444 ),
 .UNSPECIFIED., .F., .F. ) 
 B_SPLINE_CURVE_WITH_KNOTS ( ( 3, 2, 2, 2, 2, 2, 3 ),
 ( 0.5892857142857143016, 0.5928571428571428603, 0.5999999999999999778, 0.6071428571428570953, 0.6142857142857143238, 0.6214285714285714413, 0.6250000000000000000 ),
 .UNSPECIFIED. ) 
 CURVE ( )  GEOMETRIC_REPRESENTATION_ITEM ( )  RATIONAL_B_SPLINE_CURVE ( ( 0.9755282581475768211, 0.9755282581475768211, 1.000000000000000000, 0.9510565162951535312, 1.000000000000000000, 0.9510565162951535312, 1.000000000000000000, 0.9510565162951535312, 1.000000000000000000, 0.9510565162951535312, 1.000000000000000000, 0.9755282581475768211, 0.9755282581475768211 ) ) 
 REPRESENTATION_ITEM ( '' )  );
#4752 = CARTESIAN_POINT ( 'NONE',  ( 48.01140435219951996, 86.36049967264872862, 32.58608133808903773 ) ) ;
#4753 = DIRECTION ( 'NONE',  ( 0.000000000000000000, -0.000000000000000000, 1.000000000000000000 ) ) ;
#4754 = CIRCLE ( 'NONE', #17070, 10.00000000000000888 ) ;
#4755 = CARTESIAN_POINT ( 'NONE',  ( -176.9699209214867608, -136.9891397928655010, 67.64809332337415526 ) ) ;
#4756 = CARTESIAN_POINT ( 'NONE',  ( -130.4480969619997950, -126.9891397928655010, -72.64809332337412684 ) ) ;
#4757 = CARTESIAN_POINT ( 'NONE',  ( 39.42975644700377558, 90.41518717409400097, 36.81289934271958941 ) ) ;
#4758 = CARTESIAN_POINT ( 'NONE',  ( 46.10157429594899270, 107.6604996726487116, 29.95742577749336988 ) ) ;
#4759 = CARTESIAN_POINT ( 'NONE',  ( 47.05648932407426344, 142.5844580088725877, 31.27175355779120025 ) ) ;
#4760 = EDGE_LOOP ( 'NONE', ( #3128, #14818, #19148, #17206 ) ) ;
#4761 = CARTESIAN_POINT ( 'NONE',  ( 44.37947211624943833, 64.27977050742731535, 38.42115945441014446 ) ) ;
#4762 = CARTESIAN_POINT ( 'NONE',  ( -154.3824083646099439, -160.2938272943107449, 58.62277379824867296 ) ) ;
#4763 = CARTESIAN_POINT ( 'NONE',  ( 30.90322180743143576, 151.9278386122780375, 10.43433729856376502 ) ) ;
#4764 = CARTESIAN_POINT ( 'NONE',  ( -151.4692556286852891, -184.4084106276440593, 59.56931450028537967 ) ) ;
#4765 = EDGE_LOOP ( 'NONE', ( #17772, #14554 ) ) ;
#4766 = CARTESIAN_POINT ( 'NONE',  ( -159.5594255724347761, -161.1891397928654897, 55.53486410454104316 ) ) ;
#4767 = EDGE_CURVE ( 'NONE', #1030, #13261, #14987, .T. ) ;
#4768 = DIRECTION ( 'NONE',  ( 0.000000000000000000, 0.000000000000000000, 1.000000000000000000 ) ) ;
#4769 = EDGE_CURVE ( 'NONE', #1878, #255, #12607, .T. ) ;
#4770 = CARTESIAN_POINT ( 'NONE',  ( 43.01140435219951286, 128.6297705074273381, 29.55568802177586107 ) ) ;
#4771 = CARTESIAN_POINT ( 'NONE',  ( 15.39564893635072806, 140.1373336744895255, -4.208549045858890558 ) ) ;
#4772 = ORIENTED_EDGE ( 'NONE', *, *, #18909, .F. ) ;
#4773 = VECTOR ( 'NONE', #1786, 1000.000000000000000 ) ;
#4774 = CARTESIAN_POINT ( 'NONE',  ( -151.4692556286852891, -194.3130981290893260, 39.65701158161630246 ) ) ;
#4775 = VERTEX_POINT ( 'NONE', #9307 ) ;
#4776 = CARTESIAN_POINT ( 'NONE',  ( 38.58424406990784661, 117.2297705074273040, 32.77220824515698183 ) ) ;
#4777 = CARTESIAN_POINT ( 'NONE',  ( 164.7397274782390184, 67.46000011932014218, 14.00000000000001776 ) ) ;
#4778 = CARTESIAN_POINT ( 'NONE',  ( 38.58424406990784661, 155.9651871740939555, 32.77220824515698183 ) ) ;
#4779 = APPLICATION_CONTEXT ( 'automotive_design' ) ;
#4780 = VECTOR ( 'NONE', #18040, 1000.000000000000000 ) ;
#4781 = LINE ( 'NONE', #9758, #9063 ) ;
#4782 = DIRECTION ( 'NONE',  ( 0.000000000000000000, 0.000000000000000000, 1.000000000000000000 ) ) ;
#4783 = CARTESIAN_POINT ( 'NONE',  ( -161.4692556286852891, -176.3391397928654385, 52.90620854394536821 ) ) ;
#4784 = CARTESIAN_POINT ( 'NONE',  ( -143.3790856849358306, -180.6891397928654612, 43.77915905869157598 ) ) ;
#4785 = CARTESIAN_POINT ( 'NONE',  ( 43.01140435219951996, 10.71049967264875491, 29.21067981925357060 ) ) ;
#4786 = CARTESIAN_POINT ( 'NONE',  ( -160.8964159109769696, -193.7438272943106767, 52.72008163687743121 ) ) ;
#4787 = AXIS2_PLACEMENT_3D ( 'NONE', #919, #12819, #4664 ) ;
#4788 = EDGE_CURVE ( 'NONE', #3809, #17748, #3912, .T. ) ;
#4789 = CARTESIAN_POINT ( 'NONE',  ( 43.01140435219951286, 119.0344580088725621, 28.95336869806222779 ) ) ;
#4790 = CARTESIAN_POINT ( 'NONE',  ( 44.37947211624943833, 104.4797705074273182, 30.00020018409699318 ) ) ;
#4791 = CARTESIAN_POINT ( 'NONE',  ( 34.17400395940548918, 146.6865494356538875, -10.43883331896520694 ) ) ;
#4792 = CARTESIAN_POINT ( 'NONE',  ( -160.8964159109769696, -182.0438272943107449, 46.59394152635518793 ) ) ;
#4793 = CARTESIAN_POINT ( 'NONE',  ( 46.59305225739526435, 91.91518717409400097, 31.60846029578754468 ) ) ;
#4794 = LINE ( 'NONE', #21562, #16107 ) ;
#4795 = ORIENTED_EDGE ( 'NONE', *, *, #7281, .T. ) ;
#4796 = DIRECTION ( 'NONE',  ( 0.000000000000000000, 0.000000000000000000, 1.000000000000000000 ) ) ;
#4797 = PLANE ( 'NONE',  #8158 ) ;
#4798 = CARTESIAN_POINT ( 'NONE',  ( 36.80677928932056631, 92.47987693618573246, 1.660900796654692702 ) ) ;
#4799 = CARTESIAN_POINT ( 'NONE',  ( 39.42975644700377558, 66.67977050742732104, 36.81289934271958941 ) ) ;
#4800 = EDGE_LOOP ( 'NONE', ( #6765, #7173, #12032, #19175, #16521 ) ) ;
#4801 = VECTOR ( 'NONE', #1078, 1000.000000000000000 ) ;
#4802 = CARTESIAN_POINT ( 'NONE',  ( 47.43856463449117200, 146.0297705074272869, 32.77220824515698183 ) ) ;
#4803 = CIRCLE ( 'NONE', #5853, 7.500000000000007105 ) ;
#4804 = CARTESIAN_POINT ( 'NONE',  ( 40.27526882409969033, 99.82977050742729830, 37.97664729208901946 ) ) ;
#4805 = AXIS2_PLACEMENT_3D ( 'NONE', #3130, #18340, #8209 ) ;
#4806 = DIRECTION ( 'NONE',  ( 1.000000000000000000, 0.000000000000000000, 0.000000000000000000 ) ) ;
#4807 = CARTESIAN_POINT ( 'NONE',  ( 41.46631938032478359, 112.3104996726487457, 38.96596240072933170 ) ) ;
#4808 = CARTESIAN_POINT ( 'NONE',  ( 38.58424406990784661, 68.96518717409398391, 32.77220824515698183 ) ) ;
#4809 = CARTESIAN_POINT ( 'NONE',  ( 38.96631938032478359, 95.48445800887257917, 31.27175355779120025 ) ) ;
#4810 = CARTESIAN_POINT ( 'NONE',  ( -157.2955611005345986, -160.4438272943106654, 57.67623309621197336 ) ) ;
#4811 = CARTESIAN_POINT ( 'NONE',  ( -145.2889157411863437, -166.4391397928654897, 58.16351966513671812 ) ) ;
#4812 = CARTESIAN_POINT ( 'NONE',  ( -143.3790856849358306, -173.7630981290892862, 43.77915905869157598 ) ) ;
#4813 = EDGE_CURVE ( 'NONE', #9101, #15014, #17236, .T. ) ;
#4814 = CARTESIAN_POINT ( 'NONE',  ( 41.46631938032478359, 149.1844580088725820, 29.45539723777780239 ) ) ;
#4815 = CARTESIAN_POINT ( 'NONE',  ( 38.58424406990786082, 135.3797705074273381, 34.21067981925357060 ) ) ;
#4816 = CARTESIAN_POINT ( 'NONE',  ( 72.28893465744093305, 137.8051215927966382, 17.97743314940082371 ) ) ;
#4817 = AXIS2_PLACEMENT_3D ( 'NONE', #11281, #2914, #6327 ) ;
#4818 = CARTESIAN_POINT ( 'NONE',  ( 39.42975644700377558, 114.4151871740940010, 36.81289934271958941 ) ) ;
#4819 = CARTESIAN_POINT ( 'NONE',  ( -159.5594255724347761, -170.1891397928654897, 55.53486410454104316 ) ) ;
#4820 = CARTESIAN_POINT ( 'NONE',  ( 45.51148226160370314, 59.71123016864974176, 29.88059778228138086 ) ) ;
#4821 = CARTESIAN_POINT ( 'NONE',  ( 70.33053884415087964, 140.4045759698336724, 5.867304552604015733 ) ) ;
#4822 =( BOUNDED_CURVE ( )  B_SPLINE_CURVE ( 2, ( #19711, #16286, #8142, #14846, #18045, #11321, #3177, #21592, #2951, #13202, #16176, #11430, #7819 ),
 .UNSPECIFIED., .F., .F. ) 
 B_SPLINE_CURVE_WITH_KNOTS ( ( 3, 2, 2, 2, 2, 2, 3 ),
 ( 0.1964285714285714524, 0.2000000000000000111, 0.2071428571428571563, 0.2142857142857142738, 0.2214285714285714191, 0.2285714285714285643, 0.2321428571428571508 ),
 .UNSPECIFIED. ) 
 CURVE ( )  GEOMETRIC_REPRESENTATION_ITEM ( )  RATIONAL_B_SPLINE_CURVE ( ( 0.9755282581475767101, 0.9755282581475768211, 1.000000000000000000, 0.9510565162951535312, 1.000000000000000000, 0.9510565162951535312, 1.000000000000000000, 0.9510565162951535312, 1.000000000000000000, 0.9510565162951535312, 1.000000000000000000, 0.9755282581475765991, 0.9755282581475767101 ) ) 
 REPRESENTATION_ITEM ( '' )  );
#4823 = CARTESIAN_POINT ( 'NONE',  ( 17.24633477965345918, 131.3686459745448758, -4.367463884209165315 ) ) ;
#4824 = CARTESIAN_POINT ( 'NONE',  ( 43.01140435219951286, 82.46049967264873715, 39.21067981925356349 ) ) ;
#4825 = CARTESIAN_POINT ( 'NONE',  ( 43.01140435219951286, 97.12977050742732388, 38.86567161673127657 ) ) ;
#4826 = ORIENTED_EDGE ( 'NONE', *, *, #5300, .F. ) ;
#4827 = CIRCLE ( 'NONE', #16087, 10.00000000000000888 ) ;
#4828 = LINE ( 'NONE', #8146, #19281 ) ;
#4829 = EDGE_LOOP ( 'NONE', ( #2443, #18990, #4158, #18962 ) ) ;
#4830 = CARTESIAN_POINT ( 'NONE',  ( 38.96631938032478359, 84.08445800887258770, 37.14960608071593384 ) ) ;
#4831 = CYLINDRICAL_SURFACE ( 'NONE', #9491, 9.999999999999994671 ) ;
#4832 = CARTESIAN_POINT ( 'NONE',  ( 38.96631938032478359, 138.4104996726487400, 31.27175355779120025 ) ) ;
#4834 = CARTESIAN_POINT ( 'NONE',  ( 42.74273477336613780, 91.78896094402264794, 1.422757611514577247 ) ) ;
#4833 = CARTESIAN_POINT ( 'NONE',  ( 47.43856463449118621, 100.6151871740940180, 34.21067981925357060 ) ) ;
#4835 = CARTESIAN_POINT ( 'NONE',  ( 163.3401611601854029, 191.7221236944928364, 21.73429951086134082 ) ) ;
#4836 = CARTESIAN_POINT ( 'NONE',  ( -159.0959885057557983, -163.8584106276440480, 55.19815736654470584 ) ) ;
#4837 = ADVANCED_FACE ( 'NONE', ( #707 ), #7440, .F. ) ;
#4838 = CARTESIAN_POINT ( 'NONE',  ( -151.4692556286852891, -187.1438272943107108, 59.56931450028537256 ) ) ;
#4840 = FACE_OUTER_BOUND ( 'NONE', #14250, .T. ) ;
#4839 = LINE ( 'NONE', #16404, #18906 ) ;
#4841 = DIRECTION ( 'NONE',  ( 0.000000000000000000, 0.000000000000000000, 1.000000000000000000 ) ) ;
#4842 = CARTESIAN_POINT ( 'NONE',  ( 38.96631938032478359, 147.4104996726487400, 31.27175355779120025 ) ) ;
#4843 = LINE ( 'NONE', #8160, #13614 ) ;
#4844 = CARTESIAN_POINT ( 'NONE',  ( 38.58424406990784661, 63.26518717409400239, 35.64915139335016647 ) ) ;
#4845 = CARTESIAN_POINT ( 'NONE',  ( -159.5594255724347761, -184.2630981290893146, 55.53486410454104316 ) ) ;
#4846 = CARTESIAN_POINT ( 'NONE',  ( 12.03843011909301453, 134.4860913190374561, 2.577281550626734141 ) ) ;
#4847 = CARTESIAN_POINT ( 'NONE',  ( 46.59305225739526435, 148.9151871740940294, 31.60846029578754468 ) ) ;
#4848 = AXIS2_PLACEMENT_3D ( 'NONE', #8452, #5133, #170 ) ;
#4849 = CARTESIAN_POINT ( 'NONE',  ( -159.0959885057557983, -164.1938272943107222, 44.11586579668791330 ) ) ;
#4850 = CARTESIAN_POINT ( 'NONE',  ( -157.2955611005345986, -179.6084106276440480, 41.63779006702063867 ) ) ;
#4851 = ORIENTED_EDGE ( 'NONE', *, *, #5054, .T. ) ;
#4852 = CARTESIAN_POINT ( 'NONE',  ( 45.74753988029934249, 64.16518717409400097, 37.97664729208901235 ) ) ;
#4853 = CARTESIAN_POINT ( 'NONE',  ( -160.8964159109769696, -161.1584106276440593, 49.65701158161630957 ) ) ;
#4854 = CARTESIAN_POINT ( 'NONE',  ( 25.66908397218059790, 90.29788686741908066, 13.93020729814628744 ) ) ;
#4855 = VECTOR ( 'NONE', #10627, 1000.000000000000000 ) ;
#4856 = CARTESIAN_POINT ( 'NONE',  ( -141.7556754875394631, -195.8237752102547518, 49.65701158161630957 ) ) ;
#4857 = CARTESIAN_POINT ( 'NONE',  ( 43.01140435219951286, 122.3651871740939754, 29.55568802177586463 ) ) ;
#4858 = CARTESIAN_POINT ( 'NONE',  ( 11.90670198672629354, 134.0117795012786814, -10.44205992529839122 ) ) ;
#4859 = VERTEX_POINT ( 'NONE', #8327 ) ;
#4860 = VERTEX_POINT ( 'NONE', #20125 ) ;
#4861 = CARTESIAN_POINT ( 'NONE',  ( -151.4692556286852891, -190.7391397928654726, 59.65701158161632378 ) ) ;
#4862 = VERTEX_POINT ( 'NONE', #13708 ) ;
#4863 = CARTESIAN_POINT ( 'NONE',  ( 41.46631938032478359, 111.3844580088725849, 38.96596240072933170 ) ) ;
#4864 = CARTESIAN_POINT ( 'NONE',  ( 40.27526882409969744, 158.9297705074272926, 30.44471234641812174 ) ) ;
#4865 = CARTESIAN_POINT ( 'NONE',  ( 45.74753988029933538, 71.32977050742732672, 30.44471234641811819 ) ) ;
#4867 = CARTESIAN_POINT ( 'NONE',  ( 37.56771007382699423, 92.23784766911828115, 0.6328166970475824771 ) ) ;
#4866 = CARTESIAN_POINT ( 'NONE',  ( 41.64333658814960870, 126.7151871740939981, 38.42115945441014446 ) ) ;
#4868 = CARTESIAN_POINT ( 'NONE',  ( 46.10157429594899270, 79.76049967264873430, 38.46393386101376421 ) ) ;
#4869 = MECHANICAL_DESIGN_GEOMETRIC_PRESENTATION_REPRESENTATION (  '', ( #20026 ), #15063 ) ;
#4870 = FACE_BOUND ( 'NONE', #2673, .T. ) ;
#4871 = CARTESIAN_POINT ( 'NONE',  ( 39.92123440845005433, 145.1604996726486831, 38.46393386101375711 ) ) ;
#4872 = LINE ( 'NONE', #16542, #5060 ) ;
#4873 = CARTESIAN_POINT ( 'NONE',  ( 38.58424406990786082, 84.11518717409400381, 34.21067981925357060 ) ) ;
#4874 = ADVANCED_FACE ( 'NONE', ( #18571 ), #2032, .T. ) ;
#4875 = CARTESIAN_POINT ( 'NONE',  ( 40.50102589165841493, 144.7822066801371932, 29.87433574750618703 ) ) ;
#4876 = CARTESIAN_POINT ( 'NONE',  ( -161.4692556286852891, -185.6391397928654783, 46.40781461928724383 ) ) ;
#4877 = VERTEX_POINT ( 'NONE', #1709 ) ;
#4878 = CARTESIAN_POINT ( 'NONE',  ( 39.42975644700377558, 66.07977050742731251, 31.60846029578754468 ) ) ;
#4879 = CARTESIAN_POINT ( 'NONE',  ( -143.8425227516148084, -195.3584106276440480, 44.11586579668791330 ) ) ;
#4880 = CARTESIAN_POINT ( 'NONE',  ( 30.24639091383375700, 151.6717570033048048, 3.410403464249057492 ) ) ;
#4881 = CARTESIAN_POINT ( 'NONE',  ( -142.0420953463936087, -189.6584106276440593, 49.65701158161630957 ) ) ;
#4882 = ORIENTED_EDGE ( 'NONE', *, *, #1285, .T. ) ;
#4883 = CARTESIAN_POINT ( 'NONE',  ( 40.27526882409969033, 149.6651871740939725, 30.44471234641811819 ) ) ;
#4884 = CARTESIAN_POINT ( 'NONE',  ( -47.86331837773882825, -19.06233958201669765, -25.00000000000000000 ) ) ;
#4885 = CARTESIAN_POINT ( 'NONE',  ( 47.43856463449117911, 115.7297705074273324, 35.64915139335015937 ) ) ;
#4886 = CARTESIAN_POINT ( 'NONE',  ( 63.55746018358933469, 147.2895578332197033, -9.446739241148069510 ) ) ;
#4887 = ORIENTED_EDGE ( 'NONE', *, *, #20748, .F. ) ;
#4888 = CARTESIAN_POINT ( 'NONE',  ( 64.30534519084480394, 138.3942263399134447, -9.129458798097310535 ) ) ;
#4889 =( BOUNDED_CURVE ( )  B_SPLINE_CURVE ( 2, ( #9619, #14668, #21408, #13026, #19747, #18082, #9729, #16426, #6645, #227, #5088, #20297, #9945 ),
 .UNSPECIFIED., .F., .F. ) 
 B_SPLINE_CURVE_WITH_KNOTS ( ( 3, 2, 2, 2, 2, 2, 3 ),
 ( 0.4191176470588235392, 0.4205882352941176516, 0.4235294117647058765, 0.4264705882352941013, 0.4294117647058823262, 0.4323529411764706065, 0.4338235294117647189 ),
 .UNSPECIFIED. ) 
 CURVE ( )  GEOMETRIC_REPRESENTATION_ITEM ( )  RATIONAL_B_SPLINE_CURVE ( ( 0.9755282581475768211, 0.9755282581475768211, 1.000000000000000000, 0.9510565162951535312, 1.000000000000000000, 0.9510565162951535312, 1.000000000000000000, 0.9510565162951535312, 1.000000000000000000, 0.9510565162951535312, 1.000000000000000000, 0.9755282581475768211, 0.9755282581475768211 ) ) 
 REPRESENTATION_ITEM ( '' )  );
#4890 = ORIENTED_EDGE ( 'NONE', *, *, #16132, .T. ) ;
#4891 = CARTESIAN_POINT ( 'NONE',  ( 44.37947211624943833, 115.2797705074273296, 38.42115945441014446 ) ) ;
#4892 = CARTESIAN_POINT ( 'NONE',  ( 43.80332655382221674, 138.6113394311928744, 39.21067981925356349 ) ) ;
#4893 = EDGE_CURVE ( 'NONE', #15802, #17373, #2181, .T. ) ;
#4894 = CARTESIAN_POINT ( 'NONE',  ( 43.01140435219951286, 85.12977050742729546, 38.86567161673127657 ) ) ;
#4895 = CARTESIAN_POINT ( 'NONE',  ( 43.01140435219951286, 158.3651871740939612, 29.55568802177586463 ) ) ;
#4896 = CARTESIAN_POINT ( 'NONE',  ( 50.33192209904863290, 153.3481575868430014, -9.922832680162505525 ) ) ;
#4897 = CARTESIAN_POINT ( 'NONE',  ( -156.4692903108300186, -155.9898770414735623, 40.99677756761010272 ) ) ;
#4898 = LINE ( 'NONE', #17410, #18597 ) ;
#4899 = DIRECTION ( 'NONE',  ( 0.8654262854811263228, 0.000000000000000000, 0.5010362705417044094 ) ) ;
#4900 = CARTESIAN_POINT ( 'NONE',  ( -154.5594255724347761, -177.0891397928654669, 40.14644641866476604 ) ) ;
#4901 = EDGE_CURVE ( 'NONE', #13154, #4207, #12224, .T. ) ;
#4902 = CARTESIAN_POINT ( 'NONE',  ( 27.25521010731993243, 314.3399865783788414, -19.99999999999996092 ) ) ;
#4903 = CARTESIAN_POINT ( 'NONE',  ( 134.6380592378699532, 268.5785371414991687, -19.99999999999997868 ) ) ;
#4904 = CARTESIAN_POINT ( 'NONE',  ( -148.5561028927606344, -189.9938272943107336, 58.62277379824867296 ) ) ;
#4905 = ITEM_DEFINED_TRANSFORMATION ( 'NONE', 'NONE', #5978,  #12657 ) ;
#4906 = VECTOR ( 'NONE', #16157, 1000.000000000000000 ) ;
#4907 = CARTESIAN_POINT ( 'NONE',  ( 47.43856463449118621, 94.87977050742732388, 34.21067981925357060 ) ) ;
#4908 = CARTESIAN_POINT ( 'NONE',  ( 42.59292608294269655, 91.62918162712271908, 20.43785202907404752 ) ) ;
#4909 = CARTESIAN_POINT ( 'NONE',  ( -142.0420953463935803, -186.2438272943107620, 46.59394152635518793 ) ) ;
#4910 = CARTESIAN_POINT ( 'NONE',  ( 38.58424406990785371, 84.26518717409399528, 35.64915139335015937 ) ) ;
#4911 = ADVANCED_FACE ( 'NONE', ( #3687 ), #8654, .T. ) ;
#4912 = DIRECTION ( 'NONE',  ( -0.000000000000000000, -0.000000000000000000, 1.000000000000000000 ) ) ;
#4913 = ORIENTED_EDGE ( 'NONE', *, *, #6688, .F. ) ;
#4914 = CARTESIAN_POINT ( 'NONE',  ( 38.96631938032478359, 138.0844580088725877, 37.14960608071593384 ) ) ;
#4915 = CARTESIAN_POINT ( 'NONE',  ( 12.43312601512511151, 135.2277911470865490, 16.60371454366222466 ) ) ;
#4916 = CARTESIAN_POINT ( 'NONE',  ( 47.43856463449117911, 140.0297705074273154, 32.77220824515697473 ) ) ;
#4917 = CARTESIAN_POINT ( 'NONE',  ( 50.40261314387542768, 147.0381507142914188, -1.791644202716362821 ) ) ;
#4918 = CARTESIAN_POINT ( 'NONE',  ( 43.01140435219951286, 65.62977050742730967, 29.55568802177586107 ) ) ;
#4919 = ORIENTED_EDGE ( 'NONE', *, *, #21455, .F. ) ;
#4920 = CARTESIAN_POINT ( 'NONE',  ( 39.42975644700377558, 141.6797705074273210, 36.81289934271958941 ) ) ;
#4921 = EDGE_CURVE ( 'NONE', #10959, #14908, #14408, .T. ) ;
#4922 = AXIS2_PLACEMENT_3D ( 'NONE', #10433, #10650, #19233 ) ;
#4923 = CARTESIAN_POINT ( 'NONE',  ( 38.58424406990784661, 96.22977050742728977, 32.77220824515698183 ) ) ;
#4924 = CARTESIAN_POINT ( 'NONE',  ( 48.01140435219951996, 152.0604996726487457, 35.83527830041809636 ) ) ;
#4925 = ADVANCED_FACE ( 'NONE', ( #380 ), #7109, .T. ) ;
#4926 = CARTESIAN_POINT ( 'NONE',  ( 38.96631938032478359, 111.4104996726487400, 31.27175355779120025 ) ) ;
#4927 = CARTESIAN_POINT ( 'NONE',  ( 47.43856463449118621, 67.61518717409398960, 34.21067981925357060 ) ) ;
#4928 = DIRECTION ( 'NONE',  ( 0.000000000000000000, 0.000000000000000000, 1.000000000000000000 ) ) ;
#4929 = CARTESIAN_POINT ( 'NONE',  ( -151.4692556286852891, -166.1438272943107393, 59.56931450028537256 ) ) ;
#4930 = CARTESIAN_POINT ( 'NONE',  ( 177.7722984847500527, 196.9902717476302882, 21.73429951086134082 ) ) ;
#4931 = CARTESIAN_POINT ( 'NONE',  ( -151.4692556286852891, -177.8130981290892976, 60.17163382399899518 ) ) ;
#4932 = DIRECTION ( 'NONE',  ( 1.000000000000000000, 0.000000000000000000, 0.000000000000000000 ) ) ;
#4933 = CARTESIAN_POINT ( 'NONE',  ( -151.4692556286852607, -170.3130981290892692, 39.65701158161629536 ) ) ;
#4934 = CARTESIAN_POINT ( 'NONE',  ( 43.01140435219951286, 153.5344580088726048, 39.46799094044489209 ) ) ;
#4935 = CARTESIAN_POINT ( 'NONE',  ( 38.58424406990786082, 120.3797705074273239, 34.21067981925357060 ) ) ;
#4936 = CARTESIAN_POINT ( 'NONE',  ( 37.02312590732701381, 153.6946607573816834, 9.644493012478044136 ) ) ;
#4937 = CARTESIAN_POINT ( 'NONE',  ( 47.43856463449118621, 115.6151871740940038, 34.21067981925357060 ) ) ;
#4938 = CARTESIAN_POINT ( 'NONE',  ( -161.4692556286852891, -182.3391397928654385, 52.90620854394536821 ) ) ;
#4939 = CARTESIAN_POINT ( 'NONE',  ( 38.58424406990784661, 147.2297705074273324, 32.77220824515698183 ) ) ;
#4940 = DIRECTION ( 'NONE',  ( -1.000000000000000000, 0.000000000000000000, 0.000000000000000000 ) ) ;
#4941 = CARTESIAN_POINT ( 'NONE',  ( 32.47916914626341622, 146.0660553311768979, 3.489959554161691013 ) ) ;
#4942 = CARTESIAN_POINT ( 'NONE',  ( -151.4692556286852891, -196.9891397928655010, 39.65701158161630246 ) ) ;
#4943 = CARTESIAN_POINT ( 'NONE',  ( 43.01140435219951286, 94.12977050742730967, 38.86567161673127657 ) ) ;
#4944 = ORIENTED_EDGE ( 'NONE', *, *, #17744, .T. ) ;
#4945 = EDGE_CURVE ( 'NONE', #3596, #13353, #9794, .T. ) ;
#4946 = CARTESIAN_POINT ( 'NONE',  ( 48.01140435219951996, 145.4344580088725820, 32.58608133808903773 ) ) ;
#4947 = ORIENTED_EDGE ( 'NONE', *, *, #12147, .T. ) ;
#4948 = CARTESIAN_POINT ( 'NONE',  ( 38.01140435219952707, 86.78445800887257633, 34.21067981925357060 ) ) ;
#4949 = CARTESIAN_POINT ( 'NONE',  ( -151.4692556286852891, -196.9891397928655010, 49.65701158161630957 ) ) ;
#4950 = CLOSED_SHELL ( 'NONE', ( #10873, #10138, #6282, #13013, #2348, #17992, #15657, #2442, #16692, #12304, #1789, #15809, #15911, #20972, #20534, #19831, #12928, #46, #14237, #12373, #3348, #608, #2059, #18168, #20063, #1976, #21204, #19748, #15670, #15275, #194, #17379, #2473, #17286, #13109, #9879, #17618, #1092, #18235, #6306, #94, #8807, #8836, #6026, #7509 ) ) ;
#4951 = CARTESIAN_POINT ( 'NONE',  ( 41.46631938032478359, 135.1104996726487286, 29.45539723777780239 ) ) ;
#4953 = CARTESIAN_POINT ( 'NONE',  ( 71.13077487245369923, 119.9619191372588034, 6.660813687590150245 ) ) ;
#4952 = CARTESIAN_POINT ( 'NONE',  ( 43.01140435219951286, 99.86518717409400381, 38.86567161673127657 ) ) ;
#4954 = CARTESIAN_POINT ( 'NONE',  ( -145.6429501568359797, -172.1084106276439911, 57.67623309621198047 ) ) ;
#4955 = CARTESIAN_POINT ( 'NONE',  ( -154.3824083646099439, -194.4938272943107336, 40.69124936498395328 ) ) ;
#4957 = CYLINDRICAL_SURFACE ( 'NONE', #10792, 4.999999999999997335 ) ;
#4956 = CARTESIAN_POINT ( 'NONE',  ( -161.4692556286852891, -166.7130981290893317, 46.40781461928724383 ) ) ;
#4958 = CARTESIAN_POINT ( 'NONE',  ( 43.01140435219951286, 65.03445800887257633, 29.21067981925356705 ) ) ;
#4959 = CARTESIAN_POINT ( 'NONE',  ( 137.5268905834513191, 193.0332408774651185, 272.0939500981630204 ) ) ;
#4960 = CARTESIAN_POINT ( 'NONE',  ( 101.4021762516569822, 137.5714195593754710, -19.99999999999997868 ) ) ;
#4961 = CARTESIAN_POINT ( 'NONE',  ( 41.64333658814960870, 60.71518717409399102, 38.42115945441014446 ) ) ;
#4962 =( BOUNDED_CURVE ( )  B_SPLINE_CURVE ( 2, ( #10331, #1945, #11864, #8466, #1841, #3710, #13838, #8676, #15399, #5460, #3818, #295, #7026 ),
 .UNSPECIFIED., .F., .F. ) 
 B_SPLINE_CURVE_WITH_KNOTS ( ( 3, 2, 2, 2, 2, 2, 3 ),
 ( 0.4926470588235293824, 0.4941176470588235503, 0.4970588235294117752, 0.5000000000000000000, 0.5029411764705882248, 0.5058823529411764497, 0.5073529411764705621 ),
 .UNSPECIFIED. ) 
 CURVE ( )  GEOMETRIC_REPRESENTATION_ITEM ( )  RATIONAL_B_SPLINE_CURVE ( ( 0.9755282581475768211, 0.9755282581475763770, 1.000000000000000000, 0.9510565162951535312, 1.000000000000000000, 0.9510565162951535312, 1.000000000000000000, 0.9510565162951535312, 1.000000000000000000, 0.9510565162951535312, 1.000000000000000000, 0.9755282581475768211, 0.9755282581475768211 ) ) 
 REPRESENTATION_ITEM ( '' )  );
#4963 = DIRECTION ( 'NONE',  ( 0.000000000000000000, 1.000000000000000000, 0.000000000000000000 ) ) ;
#4964 = CARTESIAN_POINT ( 'NONE',  ( 10.16827731527805767, 110.2528774685086574, 8.767718578943870966 ) ) ;
#4965 = CARTESIAN_POINT ( 'NONE',  ( 39.42975644700377558, 144.4151871740940294, 36.81289934271958941 ) ) ;
#4966 = CARTESIAN_POINT ( 'NONE',  ( -154.3824083646099439, -179.7584106276440536, 40.69124936498395328 ) ) ;
#4967 = VERTEX_POINT ( 'NONE', #13917 ) ;
#4968 = CARTESIAN_POINT ( 'NONE',  ( 42.21948215057684450, 77.11133943119284595, 29.21067981925356705 ) ) ;
#4969 = CARTESIAN_POINT ( 'NONE',  ( -157.2955611005346270, -164.6084106276440764, 41.63779006702063867 ) ) ;
#4970 = CARTESIAN_POINT ( 'NONE',  ( 26.46568392313936968, 149.8720644322279725, 23.30118661649528633 ) ) ;
#4971 = CARTESIAN_POINT ( 'NONE',  ( 43.01140435219951286, 135.5344580088725763, 39.21067981925356349 ) ) ;
#4972 = CARTESIAN_POINT ( 'NONE',  ( 47.43856463449117200, 121.7651871740940237, 32.77220824515698183 ) ) ;
#4973 = CARTESIAN_POINT ( 'NONE',  ( 25.98494354700934750, 90.29984025740714060, -5.084945496952688160 ) ) ;
#4974 = ORIENTED_EDGE ( 'NONE', *, *, #10822, .F. ) ;
#4975 = VERTEX_POINT ( 'NONE', #3796 ) ;
#4976 = EDGE_CURVE ( 'NONE', #4552, #18638, #19112, .T. ) ;
#4977 = VERTEX_POINT ( 'NONE', #20658 ) ;
#4978 = CARTESIAN_POINT ( 'NONE',  ( 44.55648932407425633, 109.8844580088725849, 29.45539723777780239 ) ) ;
#4979 = PRODUCT_DEFINITION_SHAPE ( 'NONE', 'NONE',  #8803 ) ;
#4980 = CARTESIAN_POINT ( 'NONE',  ( 47.43856463449117911, 155.0297705074273438, 32.77220824515697473 ) ) ;
#4981 = CARTESIAN_POINT ( 'NONE',  ( 47.43856463449117200, 71.02977050742730114, 32.77220824515698183 ) ) ;
#4983 = CARTESIAN_POINT ( 'NONE',  ( 16.97565887011968400, 109.0741130153051444, 8.727962422049884594 ) ) ;
#4982 = CARTESIAN_POINT ( 'NONE',  ( 38.58424406990784661, 128.9651871740939839, 32.77220824515698183 ) ) ;
#4984 = EDGE_CURVE ( 'NONE', #7226, #4204, #18930, .T. ) ;
#4985 = CARTESIAN_POINT ( 'NONE',  ( 38.96631938032478359, 78.41049967264873999, 31.27175355779120025 ) ) ;
#4986 = CARTESIAN_POINT ( 'NONE',  ( 21.90415124324598750, 92.95514585177724598, 15.07745334355238676 ) ) ;
#4987 = CARTESIAN_POINT ( 'NONE',  ( -151.4692556286852607, -171.8130981290892976, 59.65701158161632378 ) ) ;
#4988 = DIRECTION ( 'NONE',  ( -0.000000000000000000, -0.000000000000000000, 1.000000000000000000 ) ) ;
#4989 = CARTESIAN_POINT ( 'NONE',  ( 46.59305225739526435, 88.31518717409400665, 36.81289934271958941 ) ) ;
#4990 = CARTESIAN_POINT ( 'NONE',  ( 39.03837758695365778, 144.5900556825055219, 37.26405200954400954 ) ) ;
#4991 = DIRECTION ( 'NONE',  ( -0.3428981916074304581, 0.9393725726208712601, 0.000000000000000000 ) ) ;
#4992 = ORIENTED_EDGE ( 'NONE', *, *, #13631, .F. ) ;
#4993 = CARTESIAN_POINT ( 'NONE',  ( 38.58424406990786082, 69.37977050742730967, 34.21067981925357060 ) ) ;
#4994 = CARTESIAN_POINT ( 'NONE',  ( -142.0420953463936087, -183.6584106276440309, 49.65701158161630957 ) ) ;
#4995 = CARTESIAN_POINT ( 'NONE',  ( 53.70366401737062034, 152.5123965792994625, -3.808113302951443568 ) ) ;
#4996 = CARTESIAN_POINT ( 'NONE',  ( -151.4692556286852891, -175.4084106276440878, 59.56931450028537967 ) ) ;
#4997 = VERTEX_POINT ( 'NONE', #10847 ) ;
#4998 = AXIS2_PLACEMENT_3D ( 'NONE', #8976, #20982, #7432 ) ;
#4999 = CARTESIAN_POINT ( 'NONE',  ( 45.74753988029933538, 158.0651871740940067, 30.44471234641811819 ) ) ;
#5000 = VECTOR ( 'NONE', #16555, 1000.000000000000000 ) ;
#5001 = CARTESIAN_POINT ( 'NONE',  ( -148.3790856849358306, -160.5891397928654953, 59.16757674456786020 ) ) ;
#5002 = CARTESIAN_POINT ( 'NONE',  ( 40.27526882409969744, 111.8297705074272983, 37.97664729208901235 ) ) ;
#5003 = CARTESIAN_POINT ( 'NONE',  ( 44.55648932407425633, 153.6844580088725820, 38.96596240072933170 ) ) ;
#5004 = EDGE_LOOP ( 'NONE', ( #8112, #1224, #12965, #21215 ) ) ;
#5005 = CARTESIAN_POINT ( 'NONE',  ( 59.92122946415073415, 142.4742691614619332, -9.367183195626855863 ) ) ;
#5006 = EDGE_LOOP ( 'NONE', ( #4357, #10188, #7668, #4493 ) ) ;
#5007 = CARTESIAN_POINT ( 'NONE',  ( 40.27526882409969033, 120.8297705074272983, 37.97664729208901946 ) ) ;
#5008 = CARTESIAN_POINT ( 'NONE',  ( 41.46631938032478359, 129.3844580088725706, 38.96596240072933170 ) ) ;
#5009 = CARTESIAN_POINT ( 'NONE',  ( 46.59305225739526435, 157.3151871740940067, 36.81289934271958941 ) ) ;
#5010 = EDGE_CURVE ( 'NONE', #8, #4022, #2138, .T. ) ;
#5011 = CARTESIAN_POINT ( 'NONE',  ( 75.85495621331871519, 129.5603373922052697, -8.732165470513974626 ) ) ;
#5012 = VECTOR ( 'NONE', #444, 1000.000000000000000 ) ;
#5013 = CARTESIAN_POINT ( 'NONE',  ( 38.01140435219952707, 107.9344580088725678, 35.83527830041809636 ) ) ;
#5014 = DIRECTION ( 'NONE',  ( -0.000000000000000000, -0.000000000000000000, 1.000000000000000000 ) ) ;
#5015 = CARTESIAN_POINT ( 'NONE',  ( 163.1026836591718734, 192.4288937294299160, 24.47866928663567521 ) ) ;
#5016 = CARTESIAN_POINT ( 'NONE',  ( -154.5594255724347761, -175.8891397928654783, 59.16757674456785310 ) ) ;
#5017 = CARTESIAN_POINT ( 'NONE',  ( 41.46631938032478359, 157.3104996726487457, 38.96596240072933170 ) ) ;
#5018 = DIRECTION ( 'NONE',  ( -0.9385982292947088190, -0.3450121214752277510, 0.000000000000000000 ) ) ;
#5019 = CARTESIAN_POINT ( 'NONE',  ( 43.01140435219951286, 92.96049967264875136, 29.21067981925356705 ) ) ;
#5020 = CARTESIAN_POINT ( 'NONE',  ( 165.8083469658213005, 192.9029763258799335, -29.99999999999997868 ) ) ;
#5021 = CARTESIAN_POINT ( 'NONE',  ( 47.43856463449117200, 91.72977050742730398, 35.64915139335016647 ) ) ;
#5022 = CARTESIAN_POINT ( 'NONE',  ( 69.25106277675128297, 109.5764507715396832, -0.9149236002526208722 ) ) ;
#5023 = CARTESIAN_POINT ( 'NONE',  ( -145.6429501568359797, -171.8438272943107279, 57.67623309621198047 ) ) ;
#5024 = CARTESIAN_POINT ( 'NONE',  ( 45.74753988029934249, 92.06518717409399244, 30.44471234641812174 ) ) ;
#5025 = CARTESIAN_POINT ( 'NONE',  ( 43.01140435219951286, 83.96049967264873715, 29.21067981925356705 ) ) ;
#5026 = ORIENTED_EDGE ( 'NONE', *, *, #6493, .F. ) ;
#5027 = CARTESIAN_POINT ( 'NONE',  ( 107.0370895198517189, 343.6663954850758955, -19.99999999999997868 ) ) ;
#5028 = CARTESIAN_POINT ( 'NONE',  ( 34.41316853928974950, 153.0433231119815503, 10.55326060710041958 ) ) ;
#5029 =( BOUNDED_CURVE ( )  B_SPLINE_CURVE ( 2, ( #17564, #4336, #11062, #4236, #15909, #20485, #17456, #15804, #7448, #2470, #17673, #4892, #2911 ),
 .UNSPECIFIED., .F., .F. ) 
 B_SPLINE_CURVE_WITH_KNOTS ( ( 3, 2, 2, 2, 2, 2, 3 ),
 ( 0.1838235294117646912, 0.1852941176470588314, 0.1882352941176470562, 0.1911764705882352811, 0.1941176470588235337, 0.1970588235294117585, 0.1985294117647058709 ),
 .UNSPECIFIED. ) 
 CURVE ( )  GEOMETRIC_REPRESENTATION_ITEM ( )  RATIONAL_B_SPLINE_CURVE ( ( 0.9755282581475765991, 0.9755282581475764880, 1.000000000000000000, 0.9510565162951535312, 1.000000000000000000, 0.9510565162951535312, 1.000000000000000000, 0.9510565162951535312, 1.000000000000000000, 0.9510565162951535312, 1.000000000000000000, 0.9755282581475769321, 0.9755282581475765991 ) ) 
 REPRESENTATION_ITEM ( '' )  );
#5030 = CARTESIAN_POINT ( 'NONE',  ( 17.19109055900979399, 108.7710072034773532, -4.291528102762561581 ) ) ;
#5031 = CARTESIAN_POINT ( 'NONE',  ( 43.01140435219951996, 10.71049967264875491, 34.21067981925357060 ) ) ;
#5032 = ORIENTED_EDGE ( 'NONE', *, *, #1437, .T. ) ;
#5033 = ADVANCED_FACE ( 'NONE', ( #10629 ), #804, .T. ) ;
#5034 = CARTESIAN_POINT ( 'NONE',  ( 46.59305225739526435, 143.1797705074273210, 31.60846029578754468 ) ) ;
#5035 = CARTESIAN_POINT ( 'NONE',  ( 46.59305225739526435, 95.17977050742732104, 31.60846029578754468 ) ) ;
#5036 = CARTESIAN_POINT ( 'NONE',  ( 43.01140435219952707, 140.9604996726487514, 29.21067981925357060 ) ) ;
#5037 = CARTESIAN_POINT ( 'NONE',  ( 39.92123440845004723, 114.2604996726487343, 29.95742577749337343 ) ) ;
#5038 = CARTESIAN_POINT ( 'NONE',  ( 43.01140435219951286, 62.36518717409399670, 29.55568802177586463 ) ) ;
#5039 = FACE_OUTER_BOUND ( 'NONE', #10933, .T. ) ;
#5040 = CARTESIAN_POINT ( 'NONE',  ( -142.0420953463935803, -162.5438272943106881, 52.72008163687743831 ) ) ;
#5041 = CARTESIAN_POINT ( 'NONE',  ( 38.01140435219952707, 122.7844580088725763, 34.21067981925357060 ) ) ;
#5042 = CARTESIAN_POINT ( 'NONE',  ( -151.4692556286852891, -173.3130981290893544, 39.14238933923362396 ) ) ;
#5043 = CARTESIAN_POINT ( 'NONE',  ( 41.46631938032478359, 153.3844580088725991, 38.96596240072933170 ) ) ;
#5044 = CARTESIAN_POINT ( 'NONE',  ( 44.37947211624943833, 127.2797705074273438, 38.42115945441014446 ) ) ;
#5045 = CARTESIAN_POINT ( 'NONE',  ( 40.68735894681399401, 154.1427111589966898, 9.763412716672732472 ) ) ;
#5046 = PLANE ( 'NONE',  #3603 ) ;
#5047 = CARTESIAN_POINT ( 'NONE',  ( 47.43856463449118621, 118.6151871740940038, 34.21067981925357060 ) ) ;
#5048 = CARTESIAN_POINT ( 'NONE',  ( -151.4692556286852891, -183.2391397928654726, 39.65701158161629536 ) ) ;
#5049 = LINE ( 'NONE', #3397, #12237 ) ;
#5050 = CARTESIAN_POINT ( 'NONE',  ( 76.97600836722278927, 116.3222765712875031, 6.700797217583226661 ) ) ;
#5051 = CARTESIAN_POINT ( 'NONE',  ( 22.10153057061799231, 100.9866247252079745, 1.346821830042071566 ) ) ;
#5052 = CARTESIAN_POINT ( 'NONE',  ( 147.5268905834513475, 193.0332408774651185, 14.00000000000001776 ) ) ;
#5053 = CARTESIAN_POINT ( 'NONE',  ( 43.01140435219951286, 85.12977050742729546, 38.86567161673127657 ) ) ;
#5054 = EDGE_CURVE ( 'NONE', #10397, #4877, #9074, .T. ) ;
#5055 = EDGE_LOOP ( 'NONE', ( #522, #9829 ) ) ;
#5056 = LINE ( 'NONE', #10130, #4475 ) ;
#5057 = ORIENTED_EDGE ( 'NONE', *, *, #13409, .T. ) ;
#5058 = CARTESIAN_POINT ( 'NONE',  ( 46.10157429594899270, 76.73445800887255075, 29.95742577749337343 ) ) ;
#5059 = CARTESIAN_POINT ( 'NONE',  ( 43.01140435219951286, 60.53445800887258343, 39.21067981925356349 ) ) ;
#5060 = VECTOR ( 'NONE', #21745, 1000.000000000000000 ) ;
#5061 = CARTESIAN_POINT ( 'NONE',  ( 46.10157429594899270, 140.6604996726486831, 29.95742577749337343 ) ) ;
#5063 = CARTESIAN_POINT ( 'NONE',  ( 33.21234449867455396, 152.6251194638087725, -9.489586336475131390 ) ) ;
#5062 = CARTESIAN_POINT ( 'NONE',  ( 45.74753988029933538, 94.16518717409400097, 37.97664729208901946 ) ) ;
#5064 = CARTESIAN_POINT ( 'NONE',  ( -157.6495955161842062, -194.9391397928654897, 41.15050349809590102 ) ) ;
#5065 = CARTESIAN_POINT ( 'NONE',  ( -157.2955611005345986, -193.4438272943106938, 57.67623309621197336 ) ) ;
#5066 = DIRECTION ( 'NONE',  ( -0.000000000000000000, -0.000000000000000000, -1.000000000000000000 ) ) ;
#5067 = CARTESIAN_POINT ( 'NONE',  ( 41.46631938032478359, 106.3104996726487457, 38.96596240072933170 ) ) ;
#5068 = CARTESIAN_POINT ( 'NONE',  ( -141.4692556286852891, -174.8391397928654669, 46.40781461928724383 ) ) ;
#5069 = CARTESIAN_POINT ( 'NONE',  ( 47.05648932407426344, 80.51049967264874851, 31.27175355779120025 ) ) ;
#5070 = CARTESIAN_POINT ( 'NONE',  ( 38.58424406990784661, 150.2297705074273040, 32.77220824515698183 ) ) ;
#5071 = CARTESIAN_POINT ( 'NONE',  ( 38.96631938032478359, 63.08445800887258059, 37.14960608071593384 ) ) ;
#5072 = CARTESIAN_POINT ( 'NONE',  ( 57.14511974427749408, 88.72838517433189054, 6.862995836283489304 ) ) ;
#5073 = CARTESIAN_POINT ( 'NONE',  ( 40.27526882409969744, 149.6651871740939725, 30.44471234641812174 ) ) ;
#5074 = CARTESIAN_POINT ( 'NONE',  ( -157.2955611005346270, -164.3438272943107279, 41.63779006702063867 ) ) ;
#5075 = CARTESIAN_POINT ( 'NONE',  ( -148.5561028927606344, -177.0584106276440366, 40.69124936498395328 ) ) ;
#5076 = EDGE_CURVE ( 'NONE', #12132, #7314, #4424, .T. ) ;
#5077 = ORIENTED_EDGE ( 'NONE', *, *, #5202, .F. ) ;
#5078 = CARTESIAN_POINT ( 'NONE',  ( 38.58424406990786082, 159.3797705074273381, 34.21067981925357060 ) ) ;
#5079 = CARTESIAN_POINT ( 'NONE',  ( -143.8425227516148084, -159.9584106276440423, 55.19815736654470584 ) ) ;
#5080 = CARTESIAN_POINT ( 'NONE',  ( 44.40591325931411859, 91.66001841764941105, -0.6336051400208910778 ) ) ;
#5081 = CARTESIAN_POINT ( 'NONE',  ( 38.01140435219952707, 134.7844580088726048, 34.21067981925357060 ) ) ;
#5082 = CARTESIAN_POINT ( 'NONE',  ( 41.64333658814960870, 126.7151871740939981, 38.42115945441014446 ) ) ;
#5083 = VERTEX_POINT ( 'NONE', #8870 ) ;
#5084 = ORIENTED_EDGE ( 'NONE', *, *, #660, .F. ) ;
#5085 = PLANE ( 'NONE',  #7827 ) ;
#5086 = ORIENTED_EDGE ( 'NONE', *, *, #4063, .F. ) ;
#5087 = CARTESIAN_POINT ( 'NONE',  ( 38.01140435219951996, 98.93445800887255359, 35.83527830041810347 ) ) ;
#5088 = CARTESIAN_POINT ( 'NONE',  ( 44.55648932407425633, 115.6104996726487428, 38.96596240072933170 ) ) ;
#5089 = CARTESIAN_POINT ( 'NONE',  ( 39.42975644700377558, 66.67977050742732104, 36.81289934271958941 ) ) ;
#5091 = CARTESIAN_POINT ( 'NONE',  ( 32.47916914626341622, 146.0660553311768979, 3.489959554161691013 ) ) ;
#5090 = CARTESIAN_POINT ( 'NONE',  ( 44.37947211624943833, 128.2151871740939839, 30.00020018409699318 ) ) ;
#5092 = AXIS2_PLACEMENT_3D ( 'NONE', #18089, #13031, #7968 ) ;
#5093 = CARTESIAN_POINT ( 'NONE',  ( 47.05648932407426344, 79.91049967264873999, 37.14960608071593384 ) ) ;
#5094 = CARTESIAN_POINT ( 'NONE',  ( 156.1725454929228079, -61.68114226949890622, 10.00000000000001599 ) ) ;
#5095 = LINE ( 'NONE', #8408, #6858 ) ;
#5096 = CARTESIAN_POINT ( 'NONE',  ( 47.43856463449117200, 76.46518717409401233, 35.64915139335016647 ) ) ;
#5097 = CARTESIAN_POINT ( 'NONE',  ( 38.76483609280177944, 144.5439415482201184, 31.56623162037504926 ) ) ;
#5098 = CARTESIAN_POINT ( 'NONE',  ( 38.01140435219952707, 132.8604996726487286, 35.83527830041809636 ) ) ;
#5099 = ADVANCED_FACE ( 'NONE', ( #20980 ), #15578, .F. ) ;
#5100 = ORIENTED_EDGE ( 'NONE', *, *, #20576, .F. ) ;
#5101 = CARTESIAN_POINT ( 'NONE',  ( 43.01140435219951286, 64.12977050742730967, 38.86567161673127657 ) ) ;
#5102 = CARTESIAN_POINT ( 'NONE',  ( -154.3824083646099439, -188.7584106276440536, 40.69124936498395328 ) ) ;
#5103 = CARTESIAN_POINT ( 'NONE',  ( 75.25890017065090376, 108.1762305904371004, -2.022566849933696620 ) ) ;
#5104 = CARTESIAN_POINT ( 'NONE',  ( -143.8425227516148084, -177.3584106276440480, 44.11586579668791330 ) ) ;
#5105 = VERTEX_POINT ( 'NONE', #7431 ) ;
#5106 = CARTESIAN_POINT ( 'NONE',  ( 41.64333658814960870, 152.5151871740940237, 30.00020018409699318 ) ) ;
#5107 = CARTESIAN_POINT ( 'NONE',  ( -56.84366818088135176, 789.5005544000622422, -3.999999999999996447 ) ) ;
#5108 = CARTESIAN_POINT ( 'NONE',  ( 38.58424406990785371, 117.2297705074273040, 32.77220824515697473 ) ) ;
#5109 = CARTESIAN_POINT ( 'NONE',  ( 10.61900875472251649, 108.8314319666055212, -5.279948415675857376 ) ) ;
#5110 = ORIENTED_EDGE ( 'NONE', *, *, #14401, .F. ) ;
#5111 = CARTESIAN_POINT ( 'NONE',  ( 60.38095089740433252, 142.1228462996803046, -2.343495028824083004 ) ) ;
#5112 = ORIENTED_EDGE ( 'NONE', *, *, #6212, .F. ) ;
#5113 = CARTESIAN_POINT ( 'NONE',  ( 46.59305225739526435, 115.5797705074273267, 36.81289934271958941 ) ) ;
#5114 = DIRECTION ( 'NONE',  ( -1.000000000000000000, 0.000000000000000000, 0.000000000000000000 ) ) ;
#5115 = CARTESIAN_POINT ( 'NONE',  ( 39.42975644700377558, 87.67977050742732104, 36.81289934271958941 ) ) ;
#5116 = CARTESIAN_POINT ( 'NONE',  ( 40.27526882409969033, 153.5651871740940067, 37.97664729208901946 ) ) ;
#5117 = CARTESIAN_POINT ( 'NONE',  ( 62.47932545177000208, 147.9683691103492436, 5.510132816154444946 ) ) ;
#5118 =( LENGTH_UNIT ( ) NAMED_UNIT ( * ) SI_UNIT ( .MILLI., .METRE. ) );
#5119 = DIRECTION ( 'NONE',  ( 0.3450121214752279175, -0.9385982292947087080, 0.000000000000000000 ) ) ;
#5120 = CARTESIAN_POINT ( 'NONE',  ( -154.5594255724347761, -183.0891397928654669, 40.14644641866476604 ) ) ;
#5121 = EDGE_CURVE ( 'NONE', #1193, #14927, #2453, .T. ) ;
#5122 = LINE ( 'NONE', #47, #8024 ) ;
#5123 = CARTESIAN_POINT ( 'NONE',  ( 116.4417310231185780, -136.9891397928655010, 49.65701158161629536 ) ) ;
#5124 = CARTESIAN_POINT ( 'NONE',  ( 43.80332655382220253, 76.53738109496900677, 39.21067981925355639 ) ) ;
#5125 = ITEM_DEFINED_TRANSFORMATION ( 'NONE', 'NONE', #11967,  #12657 ) ;
#5126 = CARTESIAN_POINT ( 'NONE',  ( 41.64333658814960870, 89.77977050742731535, 30.00020018409699318 ) ) ;
#5127 = CARTESIAN_POINT ( 'NONE',  ( 70.85748824340309682, 124.3570181999574515, -1.510321027129504889 ) ) ;
#5128 = CARTESIAN_POINT ( 'NONE',  ( -159.0959885057557983, -169.5938272943107279, 55.19815736654470584 ) ) ;
#5129 = CARTESIAN_POINT ( 'NONE',  ( 45.74753988029934249, 88.16518717409397254, 37.97664729208901235 ) ) ;
#5130 = CARTESIAN_POINT ( 'NONE',  ( -141.4692556286852891, -195.8391397928654385, 46.40781461928724383 ) ) ;
#5131 = AXIS2_PLACEMENT_3D ( 'NONE', #8025, #16594, #20044 ) ;
#5132 = VERTEX_POINT ( 'NONE', #909 ) ;
#5133 = DIRECTION ( 'NONE',  ( 0.000000000000000000, 0.000000000000000000, 1.000000000000000000 ) ) ;
#5134 = CARTESIAN_POINT ( 'NONE',  ( 10.16827731527805767, 110.2528774685086574, 8.767718578943870966 ) ) ;
#5135 = CARTESIAN_POINT ( 'NONE',  ( 39.42975644700377558, 141.0797705074273267, 31.60846029578754468 ) ) ;
#5136 = CARTESIAN_POINT ( 'NONE',  ( 61.95829188091916961, 99.12855633088805973, 0.5892133286805102399 ) ) ;
#5137 = CARTESIAN_POINT ( 'NONE',  ( 42.21948215057684450, 120.4575765865522925, 39.21067981925355639 ) ) ;
#5138 = VERTEX_POINT ( 'NONE', #7655 ) ;
#5139 = CARTESIAN_POINT ( 'NONE',  ( 43.01140435219951286, 145.1297705074273097, 38.86567161673127657 ) ) ;
#5140 = CARTESIAN_POINT ( 'NONE',  ( 43.01140435219951286, 100.1297705074273239, 38.86567161673127657 ) ) ;
#5141 = CARTESIAN_POINT ( 'NONE',  ( 0.000000000000000000, -126.9891397928655010, 0.000000000000000000 ) ) ;
#5142 = CARTESIAN_POINT ( 'NONE',  ( 38.58424406990786082, 63.11518717409400381, 34.21067981925357060 ) ) ;
#5143 = CARTESIAN_POINT ( 'NONE',  ( 24.43941541943582862, 313.3049502139530205, 4.000000000000003553 ) ) ;
#5144 = CARTESIAN_POINT ( 'NONE',  ( 43.01140435219951996, 154.4604996726487798, 39.21067981925357060 ) ) ;
#5145 = DIRECTION ( 'NONE',  ( -0.000000000000000000, -0.000000000000000000, 1.000000000000000000 ) ) ;
#5146 = CYLINDRICAL_SURFACE ( 'NONE', #15990, 10.00000000000000888 ) ;
#5147 = CARTESIAN_POINT ( 'NONE',  ( 38.96631938032478359, 141.0844580088725877, 37.14960608071593384 ) ) ;
#5148 = CARTESIAN_POINT ( 'NONE',  ( 44.37947211624943833, 119.4797705074273182, 30.00020018409699318 ) ) ;
#5149 =( BOUNDED_CURVE ( )  B_SPLINE_CURVE ( 2, ( #17774, #18107, #11170, #19440, #19771, #9857, #3127, #13157, #17881, #7986, #4333, #11058, #16233 ),
 .UNSPECIFIED., .F., .F. ) 
 B_SPLINE_CURVE_WITH_KNOTS ( ( 3, 2, 2, 2, 2, 2, 3 ),
 ( 0.6838235294117647189, 0.6852941176470588314, 0.6882352941176470562, 0.6911764705882352811, 0.6941176470588235059, 0.6970588235294117307, 0.6985294117647058432 ),
 .UNSPECIFIED. ) 
 CURVE ( )  GEOMETRIC_REPRESENTATION_ITEM ( )  RATIONAL_B_SPLINE_CURVE ( ( 0.9755282581475768211, 0.9755282581475768211, 1.000000000000000000, 0.9510565162951535312, 1.000000000000000000, 0.9510565162951535312, 1.000000000000000000, 0.9510565162951535312, 1.000000000000000000, 0.9510565162951535312, 1.000000000000000000, 0.9755282581475768211, 0.9755282581475768211 ) ) 
 REPRESENTATION_ITEM ( '' )  );
#5150 = CARTESIAN_POINT ( 'NONE',  ( 53.27251631713230040, 87.16359876908097704, 20.00146008344694337 ) ) ;
#5151 = DIRECTION ( 'NONE',  ( 0.000000000000000000, 0.000000000000000000, 1.000000000000000000 ) ) ;
#5152 = CARTESIAN_POINT ( 'NONE',  ( 47.43856463449117911, 118.4651871740939981, 35.64915139335015937 ) ) ;
#5153 = CARTESIAN_POINT ( 'NONE',  ( 38.01140435219952707, 125.9344580088725962, 35.83527830041809636 ) ) ;
#5154 = EDGE_CURVE ( 'NONE', #1337, #21594, #9213, .T. ) ;
#5155 = CARTESIAN_POINT ( 'NONE',  ( 74.11624783127615501, 105.8034190341144978, 7.057826790323951549 ) ) ;
#5156 = CARTESIAN_POINT ( 'NONE',  ( 32.38101408406643600, 93.78751416920769657, -6.153149741203968404 ) ) ;
#5157 = DIRECTION ( 'NONE',  ( -0.3450121214752276955, 0.9385982292947087080, -0.000000000000000000 ) ) ;
#5158 = CARTESIAN_POINT ( 'NONE',  ( 40.27526882409969744, 87.82977050742732672, 37.97664729208901235 ) ) ;
#5159 = VERTEX_POINT ( 'NONE', #1460 ) ;
#5160 = CARTESIAN_POINT ( 'NONE',  ( -149.8854112254399240, -168.7362167067690280, 59.65701158161632378 ) ) ;
#5161 = CARTESIAN_POINT ( 'NONE',  ( 46.10157429594899270, 70.73445800887257917, 29.95742577749337343 ) ) ;
#5162 = CARTESIAN_POINT ( 'NONE',  ( -151.4692556286852891, -196.9891397928655010, 40.65701158161630246 ) ) ;
#5164 = EDGE_CURVE ( 'NONE', #12681, #6453, #21307, .T. ) ;
#5163 = CARTESIAN_POINT ( 'NONE',  ( 39.92123440845004723, 129.2604996726487343, 29.95742577749337343 ) ) ;
#5166 = CARTESIAN_POINT ( 'NONE',  ( 74.95715479139145998, 107.8263973513541742, -14.01376907723217613 ) ) ;
#5165 = CARTESIAN_POINT ( 'NONE',  ( 38.58424406990784661, 86.96518717409398391, 32.77220824515698183 ) ) ;
#5167 = VECTOR ( 'NONE', #18512, 1000.000000000000000 ) ;
#5168 = CARTESIAN_POINT ( 'NONE',  ( -143.8425227516148084, -156.9584106276440423, 55.19815736654470584 ) ) ;
#5169 = CARTESIAN_POINT ( 'NONE',  ( -151.4692556286852891, -188.6438272943107393, 39.74470866294723947 ) ) ;
#5170 = CARTESIAN_POINT ( 'NONE',  ( -151.4692556286852891, -178.7391397928654726, 59.65701158161631668 ) ) ;
#5171 = CARTESIAN_POINT ( 'NONE',  ( 43.01140435219951286, 83.03445800887257633, 29.21067981925356705 ) ) ;
#5172 = EDGE_CURVE ( 'NONE', #8428, #14663, #1350, .T. ) ;
#5173 = CARTESIAN_POINT ( 'NONE',  ( -145.2889157411863437, -176.6130981290892805, 41.15050349809589392 ) ) ;
#5174 = LINE ( 'NONE', #13652, #5553 ) ;
#5175 = CARTESIAN_POINT ( 'NONE',  ( 39.42975644700377558, 153.6797705074273210, 36.81289934271958941 ) ) ;
#5176 = CARTESIAN_POINT ( 'NONE',  ( -153.0531000319306827, -185.2362167067690280, 39.65701158161629536 ) ) ;
#5177 = EDGE_CURVE ( 'NONE', #20168, #2045, #17869, .T. ) ;
#5178 = CARTESIAN_POINT ( 'NONE',  ( 75.59501567365037999, 109.4093883240155378, 12.93430809701916750 ) ) ;
#5179 = CARTESIAN_POINT ( 'NONE',  ( 41.64333658814960870, 146.5151871740939953, 30.00020018409699318 ) ) ;
#5180 = CARTESIAN_POINT ( 'NONE',  ( -142.0420953463936087, -162.3938272943107393, 49.65701158161630957 ) ) ;
#5181 = CARTESIAN_POINT ( 'NONE',  ( -159.0959885057557983, -173.4584106276440423, 44.11586579668791330 ) ) ;
#5182 = CARTESIAN_POINT ( 'NONE',  ( 43.01140435219951286, 60.86518717409400381, 38.86567161673127657 ) ) ;
#5183 = CARTESIAN_POINT ( 'NONE',  ( -142.0420953463935803, -162.8084106276440650, 52.72008163687743831 ) ) ;
#5184 = CARTESIAN_POINT ( 'NONE',  ( 43.42882498487155374, 148.1844126167958393, 2.937742163556189112 ) ) ;
#5185 = EDGE_CURVE ( 'NONE', #1933, #1699, #956, .T. ) ;
#5186 = CARTESIAN_POINT ( 'NONE',  ( -134.9004869860375777, 755.4811543468929358, -3.999999999999980904 ) ) ;
#5187 = CARTESIAN_POINT ( 'NONE',  ( 43.01140435219951286, 125.3651871740940180, 29.55568802177586463 ) ) ;
#5188 = AXIS2_PLACEMENT_3D ( 'NONE', #9596, #16187, #12564 ) ;
#5189 = ORIENTED_EDGE ( 'NONE', *, *, #8762, .F. ) ;
#5190 = B_SPLINE_CURVE_WITH_KNOTS ( 'NONE', 1,
 ( #16725, #6722 ),
 .UNSPECIFIED., .F., .F.,
 ( 2, 2 ),
 ( 0.000000000000000000, 1.000000000000000000 ),
 .UNSPECIFIED. ) ;
#5191 = CARTESIAN_POINT ( 'NONE',  ( 42.21948215057683740, 146.1113394311928744, 29.21067981925357415 ) ) ;
#5192 = VERTEX_POINT ( 'NONE', #3000 ) ;
#5193 = CARTESIAN_POINT ( 'NONE',  ( 43.01140435219951286, 98.03445800887257633, 28.95336869806222779 ) ) ;
#5194 = CARTESIAN_POINT ( 'NONE',  ( 45.74753988029934249, 157.4297705074273210, 37.97664729208901235 ) ) ;
#5195 = EDGE_CURVE ( 'NONE', #15871, #17093, #10626, .T. ) ;
#5196 = CARTESIAN_POINT ( 'NONE',  ( 39.42975644700377558, 60.67977050742731393, 36.81289934271958941 ) ) ;
#5198 = CARTESIAN_POINT ( 'NONE',  ( 60.04598833032897431, 142.2798636455802921, -15.36278432740704147 ) ) ;
#5197 = CARTESIAN_POINT ( 'NONE',  ( 40.27526882409969033, 120.5651871740940209, 37.97664729208901946 ) ) ;
#5199 = VECTOR ( 'NONE', #4218, 1000.000000000000000 ) ;
#5200 = CARTESIAN_POINT ( 'NONE',  ( 47.05648932407426344, 80.51049967264874851, 31.27175355779120025 ) ) ;
#5201 = CARTESIAN_POINT ( 'NONE',  ( -136.6255475934131596, 760.1741454933652449, -3.999999999999980904 ) ) ;
#5202 = EDGE_CURVE ( 'NONE', #20722, #17644, #9409, .T. ) ;
#5203 = CARTESIAN_POINT ( 'NONE',  ( -141.4692556286852891, -171.0630981290893260, 49.65701158161630957 ) ) ;
#5204 = CARTESIAN_POINT ( 'NONE',  ( -157.6495955161842062, -191.0130981290893146, 41.15050349809589392 ) ) ;
#5205 = CARTESIAN_POINT ( 'NONE',  ( 39.42975644700377558, 75.41518717409400097, 36.81289934271958941 ) ) ;
#5206 = CARTESIAN_POINT ( 'NONE',  ( 43.01140435219951996, 10.71049967264875491, 34.21067981925357060 ) ) ;
#5207 = CIRCLE ( 'NONE', #18926, 10.00000000000000888 ) ;
#5208 = CARTESIAN_POINT ( 'NONE',  ( 41.46631938032478359, 122.1844580088725962, 29.45539723777780239 ) ) ;
#5209 = CARTESIAN_POINT ( 'NONE',  ( 31.20897972572539558, 148.4098837309084900, 17.43780275515693390 ) ) ;
#5210 = ORIENTED_EDGE ( 'NONE', *, *, #12062, .F. ) ;
#5211 = CARTESIAN_POINT ( 'NONE',  ( 41.64333658814960870, 69.97977050742731819, 38.42115945441014446 ) ) ;
#5212 = CARTESIAN_POINT ( 'NONE',  ( -160.8964159109769696, -182.1584106276440309, 49.65701158161630957 ) ) ;
#5213 = CARTESIAN_POINT ( 'NONE',  ( 65.27013532398795803, 145.9152199903044504, 11.62486143609835310 ) ) ;
#5214 = CARTESIAN_POINT ( 'NONE',  ( -157.2955611005346270, -173.6084106276440480, 41.63779006702063867 ) ) ;
#5215 = VERTEX_POINT ( 'NONE', #3113 ) ;
#5216 =( REPRESENTATION_RELATIONSHIP ('NONE','NONE', #6933, #17468 ) REPRESENTATION_RELATIONSHIP_WITH_TRANSFORMATION ( #50 )SHAPE_REPRESENTATION_RELATIONSHIP( ) );
#5217 = CARTESIAN_POINT ( 'NONE',  ( 38.58424406990784661, 149.9651871740939555, 32.77220824515698183 ) ) ;
#5218 = DIRECTION ( 'NONE',  ( 0.000000000000000000, 0.000000000000000000, 1.000000000000000000 ) ) ;
#5219 = CARTESIAN_POINT ( 'NONE',  ( 46.59305225739526435, 115.5797705074273267, 36.81289934271958941 ) ) ;
#5220 = CARTESIAN_POINT ( 'NONE',  ( 76.92284642892752800, 124.5854180935290714, 5.434424407683230207 ) ) ;
#5221 = EDGE_LOOP ( 'NONE', ( #5749, #9154, #20697, #12554 ) ) ;
#5222 = CARTESIAN_POINT ( 'NONE',  ( 70.35668680342836012, 113.0167181193761508, -8.057780719902234878 ) ) ;
#5223 = ORIENTED_EDGE ( 'NONE', *, *, #17821, .T. ) ;
#5224 = CARTESIAN_POINT ( 'NONE',  ( 45.74753988029933538, 110.3297705074273125, 30.44471234641811819 ) ) ;
#5225 = CARTESIAN_POINT ( 'NONE',  ( -81.61981105773979550, 604.5992151483073940, -0.8325491102011938205 ) ) ;
#5226 = DIRECTION ( 'NONE',  ( 0.000000000000000000, 1.000000000000000000, 0.000000000000000000 ) ) ;
#5227 = CARTESIAN_POINT ( 'NONE',  ( 40.27526882409969033, 143.6651871740940294, 30.44471234641811819 ) ) ;
#5228 = CARTESIAN_POINT ( 'NONE',  ( 52.64611633815218283, 152.6728927476294189, 5.153103026933554709 ) ) ;
#5229 = DIRECTION ( 'NONE',  ( 0.5010362705417046314, -0.000000000000000000, -0.8654262854811262118 ) ) ;
#5230 = FACE_OUTER_BOUND ( 'NONE', #13458, .T. ) ;
#5231 = CARTESIAN_POINT ( 'NONE',  ( -159.5594255724347761, -179.1891397928654612, 55.53486410454104316 ) ) ;
#5232 = CARTESIAN_POINT ( 'NONE',  ( 147.8787791192428074, -136.9891397928655010, 49.65701158161629536 ) ) ;
#5233 = CARTESIAN_POINT ( 'NONE',  ( 47.05648932407426344, 77.51049967264873430, 31.27175355779120025 ) ) ;
#5234 = CARTESIAN_POINT ( 'NONE',  ( 45.74753988029933538, 98.32977050742731251, 30.44471234641811819 ) ) ;
#5235 = CARTESIAN_POINT ( 'NONE',  ( 66.49460585200260709, 135.5194395740885511, -1.986604139701473759 ) ) ;
#5236 = CARTESIAN_POINT ( 'NONE',  ( -160.8964159109769696, -172.8938272943107393, 49.65701158161630957 ) ) ;
#5237 = CARTESIAN_POINT ( 'NONE',  ( 46.59305225739526435, 76.31518717409399244, 36.81289934271958941 ) ) ;
#5238 = DIRECTION ( 'NONE',  ( -0.8302490056034136368, -0.5573926701119623628, 0.000000000000000000 ) ) ;
#5239 = CARTESIAN_POINT ( 'NONE',  ( 43.01140435219951996, 155.0344580088726048, 29.21067981925357060 ) ) ;
#5240 = ORIENTED_EDGE ( 'NONE', *, *, #315, .F. ) ;
#5241 = CARTESIAN_POINT ( 'NONE',  ( 68.01140435219951996, 119.9070776186055838, 50.00000000000002842 ) ) ;
#5242 = CARTESIAN_POINT ( 'NONE',  ( 131.9510975077307933, 193.6375880255003779, 34.00000000000001421 ) ) ;
#5243 = CARTESIAN_POINT ( 'NONE',  ( 44.37947211624943833, 143.4797705074273324, 30.00020018409699318 ) ) ;
#5244 = CARTESIAN_POINT ( 'NONE',  ( 31.68064667488295783, 94.17100518331969283, -5.125072385659846574 ) ) ;
#5245 = DIRECTION ( 'NONE',  ( 0.000000000000000000, 0.000000000000000000, 1.000000000000000000 ) ) ;
#5246 = ORIENTED_EDGE ( 'NONE', *, *, #5344, .T. ) ;
#5247 = CARTESIAN_POINT ( 'NONE',  ( 38.58424406990786082, 135.3797705074273381, 34.21067981925357060 ) ) ;
#5248 = ADVANCED_FACE ( 'NONE', ( #5976 ), #19424, .F. ) ;
#5249 = CARTESIAN_POINT ( 'NONE',  ( 38.58424406990784661, 99.22977050742731819, 32.77220824515698183 ) ) ;
#5250 = CARTESIAN_POINT ( 'NONE',  ( 43.01140435219951996, 155.9604996726487514, 29.21067981925357060 ) ) ;
#5251 = VECTOR ( 'NONE', #20916, 1000.000000000000000 ) ;
#5252 = DIRECTION ( 'NONE',  ( 0.000000000000000000, -1.000000000000000000, 0.000000000000000000 ) ) ;
#5253 = CARTESIAN_POINT ( 'NONE',  ( -154.5594255724347761, -168.9630981290893033, 59.16757674456785310 ) ) ;
#5254 = DIRECTION ( 'NONE',  ( 0.000000000000000000, -1.000000000000000000, 0.000000000000000000 ) ) ;
#5255 = LINE ( 'NONE', #5566, #8719 ) ;
#5256 = CARTESIAN_POINT ( 'NONE',  ( -154.5594255724347761, -167.1630981290892919, 40.14644641866476604 ) ) ;
#5257 = CARTESIAN_POINT ( 'NONE',  ( -32.01616736674569808, 6.938893903907228378E-15, -55.88783151651931291 ) ) ;
#5258 = CARTESIAN_POINT ( 'NONE',  ( 48.01140435219951996, 139.1344580088725706, 35.83527830041810347 ) ) ;
#5259 = CARTESIAN_POINT ( 'NONE',  ( 38.58424406990786082, 123.3797705074273239, 34.21067981925357060 ) ) ;
#5260 = CARTESIAN_POINT ( 'NONE',  ( 48.82767110959031243, 147.5835523268705458, -3.847861628839052361 ) ) ;
#5261 = CARTESIAN_POINT ( 'NONE',  ( 41.46631938032478359, 140.1844580088725820, 29.45539723777780239 ) ) ;
#5262 = CARTESIAN_POINT ( 'NONE',  ( 38.58424406990786082, 111.1151871740940038, 34.21067981925357060 ) ) ;
#5263 = EDGE_CURVE ( 'NONE', #417, #2203, #13289, .T. ) ;
#5264 = CARTESIAN_POINT ( 'NONE',  ( -143.7724355939531904, 531.4176628826018032, 4.000000000000021316 ) ) ;
#5265 = CARTESIAN_POINT ( 'NONE',  ( 21.64910689156460322, 146.5545592879464607, 4.081561387450916456 ) ) ;
#5266 = CARTESIAN_POINT ( 'NONE',  ( 41.15066532084431827, 91.76888749123396849, -6.510040445920065366 ) ) ;
#5267 = CARTESIAN_POINT ( 'NONE',  ( -149.8854112254399240, -186.7362167067690564, 59.65701158161632378 ) ) ;
#5268 = CIRCLE ( 'NONE', #6317, 10.00000000000000888 ) ;
#5269 = CARTESIAN_POINT ( 'NONE',  ( 39.42975644700377558, 81.67977050742732104, 36.81289934271958941 ) ) ;
#5270 = ORIENTED_EDGE ( 'NONE', *, *, #6973, .F. ) ;
#5271 = CARTESIAN_POINT ( 'NONE',  ( -151.4692556286852891, -196.9891397928655010, 49.65701158161630957 ) ) ;
#5272 = CARTESIAN_POINT ( 'NONE',  ( 38.01140435219951996, 68.63445800887258486, 32.58608133808903773 ) ) ;
#5273 = FACE_OUTER_BOUND ( 'NONE', #19908, .T. ) ;
#5274 = CARTESIAN_POINT ( 'NONE',  ( 41.46631938032478359, 127.3104996726487315, 38.96596240072933170 ) ) ;
#5275 = CARTESIAN_POINT ( 'NONE',  ( 47.43856463449118621, 88.61518717409400381, 34.21067981925357060 ) ) ;
#5276 = EDGE_CURVE ( 'NONE', #10216, #1227, #21197, .T. ) ;
#5277 =( BOUNDED_CURVE ( )  B_SPLINE_CURVE ( 2, ( #263, #6998, #19080, #10196, #12345, #11617, #9977, #13702, #1705, #3357, #3472, #8545, #3981 ),
 .UNSPECIFIED., .F., .F. ) 
 B_SPLINE_CURVE_WITH_KNOTS ( ( 3, 2, 2, 2, 2, 2, 3 ),
 ( 0.7426470588235294379, 0.7441176470588235503, 0.7470588235294117752, 0.7500000000000000000, 0.7529411764705882248, 0.7558823529411764497, 0.7573529411764705621 ),
 .UNSPECIFIED. ) 
 CURVE ( )  GEOMETRIC_REPRESENTATION_ITEM ( )  RATIONAL_B_SPLINE_CURVE ( ( 0.9755282581475768211, 0.9755282581475768211, 1.000000000000000000, 0.9510565162951535312, 1.000000000000000000, 0.9510565162951535312, 1.000000000000000000, 0.9510565162951535312, 1.000000000000000000, 0.9510565162951535312, 1.000000000000000000, 0.9755282581475768211, 0.9755282581475768211 ) ) 
 REPRESENTATION_ITEM ( '' )  );
#5278 = CARTESIAN_POINT ( 'NONE',  ( -148.5561028927606344, -156.0584106276440650, 40.69124936498395328 ) ) ;
#5279 = CARTESIAN_POINT ( 'NONE',  ( -142.0420953463935803, -180.5438272943107165, 52.72008163687743831 ) ) ;
#5280 = DIRECTION ( 'NONE',  ( 0.000000000000000000, 0.000000000000000000, 1.000000000000000000 ) ) ;
#5281 = CARTESIAN_POINT ( 'NONE',  ( 43.01140435219951286, 145.4604996726487229, 39.21067981925356349 ) ) ;
#5282 = CARTESIAN_POINT ( 'NONE',  ( 43.01140435219951996, 10.71049967264875491, 34.21067981925357060 ) ) ;
#5283 = CARTESIAN_POINT ( 'NONE',  ( -161.4692556286853176, -173.4891397928654726, 49.65701158161630957 ) ) ;
#5284 = CARTESIAN_POINT ( 'NONE',  ( 45.74753988029933538, 154.4297705074272926, 37.97664729208901946 ) ) ;
#5285 = CARTESIAN_POINT ( 'NONE',  ( 43.01140435219951286, 103.1297705074272955, 38.86567161673127657 ) ) ;
#5286 = CARTESIAN_POINT ( 'NONE',  ( 39.19820123626366382, 154.0079489008930693, -4.284297094604833767 ) ) ;
#5287 = CARTESIAN_POINT ( 'NONE',  ( 43.01140435219951286, 147.8651871740939896, 38.86567161673127657 ) ) ;
#5288 = DIRECTION ( 'NONE',  ( 0.000000000000000000, 1.000000000000000000, 0.000000000000000000 ) ) ;
#5289 = CARTESIAN_POINT ( 'NONE',  ( -151.4692556286852891, -175.4084106276440593, 59.56931450028537256 ) ) ;
#5290 = CARTESIAN_POINT ( 'NONE',  ( 46.59305225739526435, 61.91518717409400097, 31.60846029578754468 ) ) ;
#5291 = CARTESIAN_POINT ( 'NONE',  ( 60.26010703883354580, 142.3196469542212697, 3.652109145728902551 ) ) ;
#5292 = SURFACE_STYLE_USAGE ( .BOTH. , #18633 ) ;
#5293 = CARTESIAN_POINT ( 'NONE',  ( 46.59305225739526435, 112.3151871740940067, 36.81289934271958941 ) ) ;
#5294 = EDGE_CURVE ( 'NONE', #2224, #1138, #12811, .T. ) ;
#5295 = ORIENTED_EDGE ( 'NONE', *, *, #19202, .F. ) ;
#5296 = VERTEX_POINT ( 'NONE', #19530 ) ;
#5297 = MECHANICAL_DESIGN_GEOMETRIC_PRESENTATION_REPRESENTATION (  '', ( #18325 ), #9523 ) ;
#5298 = CARTESIAN_POINT ( 'NONE',  ( -151.4692556286853176, -193.7391397928655010, 59.65701158161632378 ) ) ;
#5299 = ORIENTED_EDGE ( 'NONE', *, *, #4637, .F. ) ;
#5300 = EDGE_CURVE ( 'NONE', #19976, #8368, #20491, .T. ) ;
#5301 = CARTESIAN_POINT ( 'NONE',  ( 48.01140435219951996, 106.4344580088725678, 32.58608133808903773 ) ) ;
#5302 = CARTESIAN_POINT ( 'NONE',  ( 47.43856463449117911, 157.7297705074273040, 35.64915139335015937 ) ) ;
#5303 = CARTESIAN_POINT ( 'NONE',  ( 41.46631938032478359, 157.3104996726487457, 38.96596240072933170 ) ) ;
#5305 = CARTESIAN_POINT ( 'NONE',  ( 23.31543935874208273, 139.7533899986231916, -16.95817871342526573 ) ) ;
#5304 = CARTESIAN_POINT ( 'NONE',  ( 47.43856463449117200, 112.7651871740940095, 32.77220824515698183 ) ) ;
#5306 = CARTESIAN_POINT ( 'NONE',  ( 48.01140435219951996, 77.21049967264873715, 34.21067981925357060 ) ) ;
#5307 = CARTESIAN_POINT ( 'NONE',  ( 43.01140435219951286, 74.03445800887257633, 29.21067981925356705 ) ) ;
#5308 = CARTESIAN_POINT ( 'NONE',  ( 41.46631938032478359, 71.18445800887258201, 29.45539723777780239 ) ) ;
#5309 = CARTESIAN_POINT ( 'NONE',  ( 44.31278541401216842, 94.93890120144995137, 29.37189892749850273 ) ) ;
#5310 = CARTESIAN_POINT ( 'NONE',  ( 39.42975644700377558, 74.81518717409399244, 31.60846029578754468 ) ) ;
#5311 = PRODUCT_DEFINITION_CONTEXT ( 'detailed design', #16172, 'design' ) ;
#5312 = CARTESIAN_POINT ( 'NONE',  ( 39.70492769379191600, 144.6885458319320321, 37.97538637126935868 ) ) ;
#5313 = CARTESIAN_POINT ( 'NONE',  ( -145.6429501568359797, -183.8438272943107563, 57.67623309621198047 ) ) ;
#5314 = FACE_OUTER_BOUND ( 'NONE', #21176, .T. ) ;
#5315 = ORIENTED_EDGE ( 'NONE', *, *, #719, .F. ) ;
#5316 = CARTESIAN_POINT ( 'NONE',  ( -145.6429501568359797, -190.1084106276440195, 57.67623309621198047 ) ) ;
#5317 = CARTESIAN_POINT ( 'NONE',  ( 14.48810111090402941, 100.9784058478479523, 15.43442115621699529 ) ) ;
#5318 = CARTESIAN_POINT ( 'NONE',  ( -159.0959885057557983, -172.8584106276440764, 55.19815736654470584 ) ) ;
#5319 = ORIENTED_EDGE ( 'NONE', *, *, #865, .T. ) ;
#5320 = CARTESIAN_POINT ( 'NONE',  ( 39.42975644700377558, 155.8151871740940067, 31.60846029578754468 ) ) ;
#5321 = DIRECTION ( 'NONE',  ( 0.3450121214752279175, -0.9385982292947087080, -0.000000000000000000 ) ) ;
#5322 = CARTESIAN_POINT ( 'NONE',  ( 39.42975644700377558, 114.0797705074273125, 31.60846029578754468 ) ) ;
#5323 = CARTESIAN_POINT ( 'NONE',  ( 11.39584491653312526, 106.7788786240791978, 8.648593811254444930 ) ) ;
#5324 = ORIENTED_EDGE ( 'NONE', *, *, #1386, .T. ) ;
#5325 = CARTESIAN_POINT ( 'NONE',  ( 53.00431643774457768, 93.53749527547704190, -6.986323292181506162 ) ) ;
#5326 = CARTESIAN_POINT ( 'NONE',  ( 41.64333658814960870, 108.9797705074273324, 38.42115945441014446 ) ) ;
#5327 = LINE ( 'NONE', #3676, #20937 ) ;
#5328 = CARTESIAN_POINT ( 'NONE',  ( 38.01140435219952707, 126.7104996726487514, 34.21067981925357060 ) ) ;
#5329 = CARTESIAN_POINT ( 'NONE',  ( 41.64333658814960870, 143.5151871740939953, 30.00020018409699318 ) ) ;
#5330 = CARTESIAN_POINT ( 'NONE',  ( 69.27296957579615366, 97.94681810169329594, -0.6368323762655749842 ) ) ;
#5331 = CARTESIAN_POINT ( 'NONE',  ( 48.01140435219951996, 119.2104996726487371, 34.21067981925357060 ) ) ;
#5332 = CARTESIAN_POINT ( 'NONE',  ( -161.4692556286852607, -167.6391397928654783, 46.40781461928724383 ) ) ;
#5333 = CARTESIAN_POINT ( 'NONE',  ( 44.55648932407425633, 100.6104996726487286, 38.96596240072933170 ) ) ;
#5334 = CARTESIAN_POINT ( 'NONE',  ( -97.23064952102208736, 13.78046159333444720, 4.000000000000021316 ) ) ;
#5335 = CARTESIAN_POINT ( 'NONE',  ( 111.4021762516569964, 137.5714195593754710, 14.00000000000001776 ) ) ;
#5336 = LINE ( 'NONE', #7004, #12375 ) ;
#5337 = CARTESIAN_POINT ( 'NONE',  ( 38.58424406990784661, 99.22977050742731819, 32.77220824515698183 ) ) ;
#5338 = CARTESIAN_POINT ( 'NONE',  ( 64.30534519084480394, 138.3942263399134447, -9.129458798097310535 ) ) ;
#5339 = CARTESIAN_POINT ( 'NONE',  ( -142.0420953463935803, -174.5438272943107449, 52.72008163687743831 ) ) ;
#5340 = CARTESIAN_POINT ( 'NONE',  ( 43.01140435219951286, 81.86518717409398960, 38.86567161673127657 ) ) ;
#5341 = CARTESIAN_POINT ( 'NONE',  ( -157.6495955161842062, -170.9391397928654328, 41.15050349809589392 ) ) ;
#5342 = CARTESIAN_POINT ( 'NONE',  ( -157.6495955161842062, -158.0391397928654271, 58.16351966513671812 ) ) ;
#5343 = EDGE_LOOP ( 'NONE', ( #2249, #2711, #19439, #8501 ) ) ;
#5344 = EDGE_CURVE ( 'NONE', #5609, #497, #9420, .T. ) ;
#5345 = EDGE_CURVE ( 'NONE', #1699, #16648, #2004, .T. ) ;
#5346 = CARTESIAN_POINT ( 'NONE',  ( -153.0531000319306827, -176.2362167067690280, 39.65701158161630957 ) ) ;
#5347 = CARTESIAN_POINT ( 'NONE',  ( 43.01140435219951996, 10.71049967264875491, 34.21067981925357060 ) ) ;
#5348 = CARTESIAN_POINT ( 'NONE',  ( 42.05360093099289287, 148.0107091728485500, 4.874927614337289938 ) ) ;
#5349 = ORIENTED_EDGE ( 'NONE', *, *, #13990, .F. ) ;
#5350 = CARTESIAN_POINT ( 'NONE',  ( 40.27526882409969744, 60.82977050742731251, 37.97664729208901235 ) ) ;
#5351 = ORIENTED_EDGE ( 'NONE', *, *, #2945, .F. ) ;
#5352 = CARTESIAN_POINT ( 'NONE',  ( 38.58424406990784661, 135.5297705074273154, 35.64915139335016647 ) ) ;
#5353 = VECTOR ( 'NONE', #2562, 1000.000000000000000 ) ;
#5354 = VECTOR ( 'NONE', #4513, 1000.000000000000000 ) ;
#5355 = CYLINDRICAL_SURFACE ( 'NONE', #17479, 10.00000000000000888 ) ;
#5356 = CARTESIAN_POINT ( 'NONE',  ( 24.43941541943582862, 313.3049502139530205, -19.99999999999997868 ) ) ;
#5357 = CARTESIAN_POINT ( 'NONE',  ( -19.70755683829218796, -31.26594044116892590, -19.99999999999997868 ) ) ;
#5358 = CARTESIAN_POINT ( 'NONE',  ( 47.43856463449117200, 100.4651871740939839, 35.64915139335016647 ) ) ;
#5359 = CARTESIAN_POINT ( 'NONE',  ( -154.3824083646099439, -155.4938272943107052, 40.69124936498395328 ) ) ;
#5360 = CARTESIAN_POINT ( 'NONE',  ( 39.92123440845005433, 123.2344580088725792, 38.46393386101375711 ) ) ;
#5361 = CARTESIAN_POINT ( 'NONE',  ( -161.4692556286852607, -169.4130981290893203, 52.90620854394536821 ) ) ;
#5362 = DIRECTION ( 'NONE',  ( 0.7999999999999990452, -2.775557561562891351E-17, -0.6000000000000013101 ) ) ;
#5363 = CARTESIAN_POINT ( 'NONE',  ( 44.55648932407425633, 141.6844580088725820, 38.96596240072933170 ) ) ;
#5364 = CARTESIAN_POINT ( 'NONE',  ( 40.27526882409969033, 125.9297705074273352, 30.44471234641811819 ) ) ;
#5365 = CARTESIAN_POINT ( 'NONE',  ( 39.80927132972225024, 148.0054509460111660, -4.205104553811644941 ) ) ;
#5366 = CARTESIAN_POINT ( 'NONE',  ( -141.4692556286852891, -183.9891397928654726, 49.65701158161630957 ) ) ;
#5367 = CARTESIAN_POINT ( 'NONE',  ( 45.74753988029934249, 106.1651871740940152, 37.97664729208901235 ) ) ;
#5368 = EDGE_CURVE ( 'NONE', #16231, #17982, #15120, .T. ) ;
#5369 = CARTESIAN_POINT ( 'NONE',  ( 43.01140435219951286, 98.96049967264873715, 29.21067981925356705 ) ) ;
#5370 = CARTESIAN_POINT ( 'NONE',  ( 68.88151390383544026, 142.3271613368909811, -9.208263745312144977 ) ) ;
#5371 = CARTESIAN_POINT ( 'NONE',  ( 63.85057544308668298, 100.9084186779620609, 13.48995955233852229 ) ) ;
#5372 = CARTESIAN_POINT ( 'NONE',  ( -149.8854112254399240, -156.7362167067690280, 59.65701158161632378 ) ) ;
#5373 = CARTESIAN_POINT ( 'NONE',  ( 39.42975644700377558, 90.67977050742732104, 36.81289934271958941 ) ) ;
#5374 = EDGE_LOOP ( 'NONE', ( #20914, #1325, #7393, #12040 ) ) ;
#5375 = CYLINDRICAL_SURFACE ( 'NONE', #20645, 10.00000000000000888 ) ;
#5376 = CARTESIAN_POINT ( 'NONE',  ( 44.55648932407425633, 75.68445800887258201, 38.96596240072933170 ) ) ;
#5377 = CARTESIAN_POINT ( 'NONE',  ( 42.21948215057684450, 59.11133943119284595, 29.21067981925356705 ) ) ;
#5378 = CARTESIAN_POINT ( 'NONE',  ( 41.46631938032478359, 130.3104996726487457, 38.96596240072933170 ) ) ;
#5380 = CARTESIAN_POINT ( 'NONE',  ( 54.06307869441068448, 152.2224424482157303, -15.79932498977872868 ) ) ;
#5379 = CARTESIAN_POINT ( 'NONE',  ( 46.59305225739526435, 88.31518717409400665, 36.81289934271958941 ) ) ;
#5381 = CARTESIAN_POINT ( 'NONE',  ( -143.8425227516148084, -159.3584106276440480, 44.11586579668791330 ) ) ;
#5382 = CARTESIAN_POINT ( 'NONE',  ( -160.8964159109769696, -179.0438272943107449, 46.59394152635518083 ) ) ;
#5383 = CARTESIAN_POINT ( 'NONE',  ( -149.8854112254399240, -177.3160212151857138, 39.65701158161629536 ) ) ;
#5384 = CARTESIAN_POINT ( 'NONE',  ( 48.01140435219951996, 127.4344580088725962, 32.58608133808903773 ) ) ;
#5385 = CARTESIAN_POINT ( 'NONE',  ( -81.10645082872859746, 10.96617311717548837, -19.99999999999997868 ) ) ;
#5386 = FACE_OUTER_BOUND ( 'NONE', #21106, .T. ) ;
#5387 = LINE ( 'NONE', #10360, #15011 ) ;
#5388 = CARTESIAN_POINT ( 'NONE',  ( 39.42975644700377558, 150.6797705074273210, 36.81289934271958941 ) ) ;
#5389 = CARTESIAN_POINT ( 'NONE',  ( 38.58424406990784661, 102.5297705074273154, 35.64915139335016647 ) ) ;
#5390 = CARTESIAN_POINT ( 'NONE',  ( 77.07719282571002850, 116.5297446719512209, 12.69640610750513865 ) ) ;
#5391 = CARTESIAN_POINT ( 'NONE',  ( 38.58424406990786082, 138.1151871740940180, 34.21067981925357060 ) ) ;
#5392 = CARTESIAN_POINT ( 'NONE',  ( -151.4692556286852607, -165.8130981290893260, 59.65701158161632378 ) ) ;
#5393 = CARTESIAN_POINT ( 'NONE',  ( -148.5561028927606344, -166.2584106276440536, 58.62277379824867296 ) ) ;
#5394 = DIRECTION ( 'NONE',  ( -0.000000000000000000, 1.000000000000000000, -0.000000000000000000 ) ) ;
#5395 = CARTESIAN_POINT ( 'NONE',  ( 12.26432857192422432, 135.0705202968918570, 22.59931835930844457 ) ) ;
#5396 = CARTESIAN_POINT ( 'NONE',  ( 41.64333658814960870, 116.5151871740940095, 30.00020018409699318 ) ) ;
#5397 = ORIENTED_EDGE ( 'NONE', *, *, #6235, .T. ) ;
#5398 = CARTESIAN_POINT ( 'NONE',  ( -161.4692556286852891, -179.6391397928654783, 46.40781461928724383 ) ) ;
#5399 = ORIENTED_EDGE ( 'NONE', *, *, #19804, .T. ) ;
#5400 =( BOUNDED_CURVE ( )  B_SPLINE_CURVE ( 2, ( #12295, #7140, #8903, #6923, #16931, #15508, #20259, #1952, #16825, #8682, #15180, #13844, #302 ),
 .UNSPECIFIED., .F., .T. ) 
 B_SPLINE_CURVE_WITH_KNOTS ( ( 3, 2, 2, 2, 2, 2, 3 ),
 ( 0.5661764705882352811, 0.5676470588235293935, 0.5705882352941176183, 0.5735294117647058432, 0.5764705882352940680, 0.5794117647058824039, 0.5808823529411765163 ),
 .UNSPECIFIED. ) 
 CURVE ( )  GEOMETRIC_REPRESENTATION_ITEM ( )  RATIONAL_B_SPLINE_CURVE ( ( 0.9755282581475768211, 0.9755282581475768211, 1.000000000000000000, 0.9510565162951535312, 1.000000000000000000, 0.9510565162951535312, 1.000000000000000000, 0.9510565162951535312, 1.000000000000000000, 0.9510565162951535312, 1.000000000000000000, 0.9755282581475768211, 0.9755282581475768211 ) ) 
 REPRESENTATION_ITEM ( '' )  );
#5401 = CARTESIAN_POINT ( 'NONE',  ( 47.05648932407426344, 96.98445800887257917, 37.14960608071593384 ) ) ;
#5402 = CARTESIAN_POINT ( 'NONE',  ( 46.10157429594899270, 155.6604996726487116, 29.95742577749337343 ) ) ;
#5404 = CARTESIAN_POINT ( 'NONE',  ( 70.51576897149806200, 126.1317638695992116, 12.41827883020830470 ) ) ;
#5403 = CARTESIAN_POINT ( 'NONE',  ( 46.59305225739526435, 112.3151871740940067, 36.81289934271958941 ) ) ;
#5405 = CARTESIAN_POINT ( 'NONE',  ( 38.96631938032478359, 73.01049967264873430, 37.14960608071593384 ) ) ;
#5407 = CARTESIAN_POINT ( 'NONE',  ( 43.80332655382220253, 136.9575765865523067, 29.21067981925356705 ) ) ;
#5406 = CARTESIAN_POINT ( 'NONE',  ( 43.01140435219951996, 144.9070776186055696, 29.21067981925357060 ) ) ;
#5408 = CARTESIAN_POINT ( 'NONE',  ( -154.5594255724347761, -173.1630981290893203, 40.14644641866476604 ) ) ;
#5409 = DIRECTION ( 'NONE',  ( 0.000000000000000000, -1.000000000000000000, 0.000000000000000000 ) ) ;
#5410 = CARTESIAN_POINT ( 'NONE',  ( 46.59305225739526435, 79.91518717409400097, 31.60846029578754468 ) ) ;
#5411 = CARTESIAN_POINT ( 'NONE',  ( 39.92123440845005433, 63.26049967264874141, 29.95742577749336988 ) ) ;
#5412 = CARTESIAN_POINT ( 'NONE',  ( -159.0959885057557983, -184.5938272943107279, 55.19815736654470584 ) ) ;
#5413 = PLANE ( 'NONE',  #67 ) ;
#5414 = ORIENTED_EDGE ( 'NONE', *, *, #6178, .F. ) ;
#5415 = CARTESIAN_POINT ( 'NONE',  ( -142.0420953463936087, -186.6584106276440309, 49.65701158161630957 ) ) ;
#5416 = CARTESIAN_POINT ( 'NONE',  ( 19.13088699441526686, 95.37848931739559077, 15.19637875606281341 ) ) ;
#5417 = AXIS2_PLACEMENT_3D ( 'NONE', #4597, #10012, #13315 ) ;
#5418 = ORIENTED_EDGE ( 'NONE', *, *, #19865, .F. ) ;
#5419 = CARTESIAN_POINT ( 'NONE',  ( 46.59305225739526435, 148.3151871740940067, 36.81289934271958941 ) ) ;
#5420 = CARTESIAN_POINT ( 'NONE',  ( 47.43856463449118621, 157.6151871740940180, 34.21067981925357060 ) ) ;
#5421 = CARTESIAN_POINT ( 'NONE',  ( 47.43856463449117911, 100.7297705074273040, 35.64915139335015937 ) ) ;
#5422 = CARTESIAN_POINT ( 'NONE',  ( 10.91571581598819662, 131.8149664739095783, 9.482090752819161139 ) ) ;
#5423 = EDGE_LOOP ( 'NONE', ( #15077, #1825, #19914, #11826 ) ) ;
#5424 = CARTESIAN_POINT ( 'NONE',  ( 70.74141321743030630, 114.7826485538520416, 5.870819564965037429 ) ) ;
#5425 = ORIENTED_EDGE ( 'NONE', *, *, #6726, .T. ) ;
#5426 = LINE ( 'NONE', #13698, #10189 ) ;
#5427 = CARTESIAN_POINT ( 'NONE',  ( 38.96631938032478359, 129.0844580088725877, 37.14960608071593384 ) ) ;
#5428 = CARTESIAN_POINT ( 'NONE',  ( 45.74753988029933538, 146.0651871740940067, 30.44471234641811819 ) ) ;
#5429 = CARTESIAN_POINT ( 'NONE',  ( 38.96631938032478359, 100.0104996726487485, 37.14960608071593384 ) ) ;
#5430 = CARTESIAN_POINT ( 'NONE',  ( 20.75180444880664510, 93.89949152720284076, -5.875022464008872625 ) ) ;
#5431 = CARTESIAN_POINT ( 'NONE',  ( 43.01140435219951286, 118.4604996726487371, 39.21067981925356349 ) ) ;
#5432 = CARTESIAN_POINT ( 'NONE',  ( -145.2889157411863721, -166.4391397928654612, 58.16351966513671812 ) ) ;
#5433 = CARTESIAN_POINT ( 'NONE',  ( -161.4692556286853176, -181.5630981290892976, 49.65701158161630957 ) ) ;
#5434 = LINE ( 'NONE', #5123, #13226 ) ;
#5435 = DIRECTION ( 'NONE',  ( 0.000000000000000000, 0.000000000000000000, 1.000000000000000000 ) ) ;
#5436 = CARTESIAN_POINT ( 'NONE',  ( -23.27144139456156324, -18.88988604584387332, -19.99999999999997868 ) ) ;
#5437 = EDGE_CURVE ( 'NONE', #175, #10216, #6533, .T. ) ;
#5438 = CARTESIAN_POINT ( 'NONE',  ( 43.01140435219951286, 80.62977050742732388, 29.55568802177586463 ) ) ;
#5439 = CARTESIAN_POINT ( 'NONE',  ( 70.84063976188440392, 115.3547488198113200, -1.153064885589385025 ) ) ;
#5440 = CARTESIAN_POINT ( 'NONE',  ( -157.2955611005346270, -178.4438272943107222, 57.67623309621198047 ) ) ;
#5441 = EDGE_CURVE ( 'NONE', #3067, #18126, #11441, .T. ) ;
#5442 = AXIS2_PLACEMENT_3D ( 'NONE', #20150, #1402, #21468 ) ;
#5443 = CARTESIAN_POINT ( 'NONE',  ( 45.74753988029934249, 79.16518717409398675, 37.97664729208901235 ) ) ;
#5444 = CARTESIAN_POINT ( 'NONE',  ( -151.4692556286852607, -169.7391397928654442, 59.65701158161632378 ) ) ;
#5445 = DIRECTION ( 'NONE',  ( 0.3450121214752278065, -0.9385982292947087080, -0.000000000000000000 ) ) ;
#5446 = ORIENTED_EDGE ( 'NONE', *, *, #9283, .T. ) ;
#5447 = CARTESIAN_POINT ( 'NONE',  ( 44.55648932407425633, 84.68445800887256780, 38.96596240072933170 ) ) ;
#5448 = CARTESIAN_POINT ( 'NONE',  ( 38.58424406990786082, 132.3797705074273381, 34.21067981925357060 ) ) ;
#5449 = CARTESIAN_POINT ( 'NONE',  ( 39.64555921537804295, 153.8934876517313342, -16.27550955686750456 ) ) ;
#5450 = ORIENTED_EDGE ( 'NONE', *, *, #15045, .F. ) ;
#5451 = CARTESIAN_POINT ( 'NONE',  ( 39.92123440845005433, 120.2344580088725650, 38.46393386101375711 ) ) ;
#5452 = VERTEX_POINT ( 'NONE', #3451 ) ;
#5453 = CARTESIAN_POINT ( 'NONE',  ( 38.58424406990784661, 132.2297705074272756, 32.77220824515698183 ) ) ;
#5454 = CARTESIAN_POINT ( 'NONE',  ( 40.27526882409969033, 92.92977050742729261, 30.44471234641811819 ) ) ;
#5455 = CARTESIAN_POINT ( 'NONE',  ( 39.42975644700377558, 60.41518717409400097, 36.81289934271958941 ) ) ;
#5456 = CARTESIAN_POINT ( 'NONE',  ( -143.3790856849358306, -192.3630981290893089, 55.53486410454105027 ) ) ;
#5457 = SHAPE_REPRESENTATION ( 'Cast Steel Heavy Body Block', ( #12657 ), #7388 ) ;
#5458 = CARTESIAN_POINT ( 'NONE',  ( 39.42975644700377558, 93.41518717409400097, 36.81289934271958941 ) ) ;
#5459 = FACE_BOUND ( 'NONE', #3115, .T. ) ;
#5460 = CARTESIAN_POINT ( 'NONE',  ( 39.92123440845005433, 108.2604996726487485, 29.95742577749336988 ) ) ;
#5461 = CARTESIAN_POINT ( 'NONE',  ( -151.4692556286852891, -171.8130981290893260, 60.17163382399899518 ) ) ;
#5462 = VECTOR ( 'NONE', #1179, 1000.000000000000000 ) ;
#5463 = CARTESIAN_POINT ( 'NONE',  ( 43.01140435219951286, 144.5344580088726048, 39.46799094044489209 ) ) ;
#5464 = CARTESIAN_POINT ( 'NONE',  ( 44.37947211624943833, 109.2797705074273154, 38.42115945441014446 ) ) ;
#5465 = CARTESIAN_POINT ( 'NONE',  ( 19.22998607435487273, 95.16999353120945671, 21.19198650444592857 ) ) ;
#5466 = CARTESIAN_POINT ( 'NONE',  ( -143.3790856849358306, -184.2891397928654840, 55.53486410454105027 ) ) ;
#5467 = CARTESIAN_POINT ( 'NONE',  ( 47.43856463449117911, 106.4651871740940123, 35.64915139335015937 ) ) ;
#5468 = VERTEX_POINT ( 'NONE', #13363 ) ;
#5469 = DIRECTION ( 'NONE',  ( -0.000000000000000000, -0.000000000000000000, -1.000000000000000000 ) ) ;
#5470 = CARTESIAN_POINT ( 'NONE',  ( 8.779377865064803999, 119.6051361893432130, -4.922546661887801100 ) ) ;
#5471 = CARTESIAN_POINT ( 'NONE',  ( 56.80456144658707274, 95.31062238922963559, 13.84685026556700116 ) ) ;
#5472 = CARTESIAN_POINT ( 'NONE',  ( 43.01140435219951286, 69.53445800887257633, 39.21067981925356349 ) ) ;
#5473 = CARTESIAN_POINT ( 'NONE',  ( 44.37947211624943833, 89.47977050742731819, 30.00020018409699318 ) ) ;
#5474 = ORIENTED_EDGE ( 'NONE', *, *, #8762, .T. ) ;
#5475 = VECTOR ( 'NONE', #2031, 1000.000000000000114 ) ;
#5476 = CARTESIAN_POINT ( 'NONE',  ( 41.46631938032478359, 71.18445800887258201, 29.45539723777780239 ) ) ;
#5477 = CARTESIAN_POINT ( 'NONE',  ( -148.3790856849358306, -171.3891397928654499, 40.14644641866477315 ) ) ;
#5478 = ADVANCED_FACE ( 'NONE', ( #15006 ), #20308, .T. ) ;
#5479 = CARTESIAN_POINT ( 'NONE',  ( 43.01140435219951286, 131.9604996726487229, 28.95336869806222779 ) ) ;
#5481 = CARTESIAN_POINT ( 'NONE',  ( 23.45433402446531446, 147.8217840461813068, -16.84717431919864339 ) ) ;
#5480 = CARTESIAN_POINT ( 'NONE',  ( 47.43856463449117200, 91.76518717409400949, 32.77220824515698183 ) ) ;
#5482 = CARTESIAN_POINT ( 'NONE',  ( -141.4692556286852891, -195.8391397928654101, 46.40781461928724383 ) ) ;
#5483 = CARTESIAN_POINT ( 'NONE',  ( -142.0420953463935803, -180.2438272943107052, 46.59394152635518083 ) ) ;
#5484 = CARTESIAN_POINT ( 'NONE',  ( 42.21948215057684450, 116.1113394311928602, 29.21067981925356705 ) ) ;
#5485 = CARTESIAN_POINT ( 'NONE',  ( 48.01140435219951996, 127.2844580088725905, 34.21067981925357060 ) ) ;
#5486 = LINE ( 'NONE', #1866, #2344 ) ;
#5487 = CARTESIAN_POINT ( 'NONE',  ( 46.59305225739526435, 139.5797705074273267, 36.81289934271958941 ) ) ;
#5488 = CARTESIAN_POINT ( 'NONE',  ( 46.59305225739526435, 104.1797705074273210, 31.60846029578754468 ) ) ;
#5489 = CARTESIAN_POINT ( 'NONE',  ( 72.33162239183086228, 137.5781058455011703, 11.98183203572534872 ) ) ;
#5490 = CARTESIAN_POINT ( 'NONE',  ( 44.37947211624943833, 134.2151871740940123, 30.00020018409699318 ) ) ;
#5491 = CARTESIAN_POINT ( 'NONE',  ( -151.4692556286852891, -187.7391397928655010, 59.65701158161632378 ) ) ;
#5492 = CARTESIAN_POINT ( 'NONE',  ( -160.8964159109769696, -167.3084106276440366, 46.59394152635518083 ) ) ;
#5493 = VECTOR ( 'NONE', #16535, 1000.000000000000000 ) ;
#5494 = CARTESIAN_POINT ( 'NONE',  ( 18.67254549292281496, -61.68114226949890622, 20.00000000000001776 ) ) ;
#5495 = CARTESIAN_POINT ( 'NONE',  ( 55.43026649837064213, 94.49908577724413306, 5.913859291446645905 ) ) ;
#5496 = FACE_OUTER_BOUND ( 'NONE', #13048, .T. ) ;
#5497 = CIRCLE ( 'NONE', #16044, 7.500000000000000000 ) ;
#5498 = CARTESIAN_POINT ( 'NONE',  ( 38.58424406990786082, 111.1151871740940038, 34.21067981925357060 ) ) ;
#5499 = ORIENTED_EDGE ( 'NONE', *, *, #12715, .F. ) ;
#5500 = CARTESIAN_POINT ( 'NONE',  ( 173.3794444120442506, -126.9891397928655010, 67.64809332337412684 ) ) ;
#5501 = ORIENTED_EDGE ( 'NONE', *, *, #8819, .T. ) ;
#5502 = CARTESIAN_POINT ( 'NONE',  ( 43.01140435219951286, 104.0344580088725763, 28.95336869806222779 ) ) ;
#5503 = VECTOR ( 'NONE', #16954, 1000.000000000000000 ) ;
#5504 = CARTESIAN_POINT ( 'NONE',  ( 41.64333658814960870, 147.9797705074273324, 38.42115945441014446 ) ) ;
#5506 = CARTESIAN_POINT ( 'NONE',  ( 65.44800906011916197, 136.9904114405718758, 11.94221925691594777 ) ) ;
#5505 = CARTESIAN_POINT ( 'NONE',  ( 40.27526882409969033, 119.6651871740939868, 30.44471234641811819 ) ) ;
#5507 = MECHANICAL_DESIGN_GEOMETRIC_PRESENTATION_REPRESENTATION (  '', ( #2689 ), #15910 ) ;
#5508 = CARTESIAN_POINT ( 'NONE',  ( 43.01140435219951286, 70.46049967264873715, 39.46799094044489209 ) ) ;
#5510 = CARTESIAN_POINT ( 'NONE',  ( 38.01140435219952707, 74.93445800887258201, 35.83527830041809636 ) ) ;
#5509 = CARTESIAN_POINT ( 'NONE',  ( 91.17254549292282206, -61.68114226949890622, 30.00000000000000000 ) ) ;
#5511 = CARTESIAN_POINT ( 'NONE',  ( 43.01140435219951996, 94.90707761860558378, 29.21067981925357060 ) ) ;
#5512 = CARTESIAN_POINT ( 'NONE',  ( 47.43856463449118621, 82.61518717409398960, 34.21067981925357060 ) ) ;
#5513 = CARTESIAN_POINT ( 'NONE',  ( 38.96631938032478359, 64.01049967264873430, 37.14960608071593384 ) ) ;
#5514 = CARTESIAN_POINT ( 'NONE',  ( -159.0959885057557983, -179.1938272943107506, 44.11586579668791330 ) ) ;
#5515 = CARTESIAN_POINT ( 'NONE',  ( -148.5561028927606344, -195.0584106276440650, 40.69124936498395328 ) ) ;
#5516 = VERTEX_POINT ( 'NONE', #10279 ) ;
#5517 = CARTESIAN_POINT ( 'NONE',  ( -148.5561028927606344, -181.2584106276440536, 58.62277379824867296 ) ) ;
#5518 = AXIS2_PLACEMENT_3D ( 'NONE', #21715, #19723, #2964 ) ;
#5519 = CARTESIAN_POINT ( 'NONE',  ( 20.86407471411557779, 93.69780688484533471, 0.1205864258981524662 ) ) ;
#5520 = ORIENTED_EDGE ( 'NONE', *, *, #11962, .T. ) ;
#5521 = CARTESIAN_POINT ( 'NONE',  ( 47.43856463449118621, 148.6151871740939896, 34.21067981925357060 ) ) ;
#5522 = FACE_OUTER_BOUND ( 'NONE', #18331, .T. ) ;
#5523 =( BOUNDED_CURVE ( )  B_SPLINE_CURVE ( 2, ( #18349, #12950, #1048, #6107, #19671, #18237, #3138, #16568, #19899, #12836, #4450, #1487, #19554 ),
 .UNSPECIFIED., .F., .F. ) 
 B_SPLINE_CURVE_WITH_KNOTS ( ( 3, 2, 2, 2, 2, 2, 3 ),
 ( 0.6250000000000000000, 0.6264705882352941124, 0.6294117647058823373, 0.6323529411764705621, 0.6352941176470587870, 0.6382352941176470118, 0.6397058823529411242 ),
 .UNSPECIFIED. ) 
 CURVE ( )  GEOMETRIC_REPRESENTATION_ITEM ( )  RATIONAL_B_SPLINE_CURVE ( ( 0.9755282581475768211, 0.9755282581475768211, 1.000000000000000000, 0.9510565162951535312, 1.000000000000000000, 0.9510565162951535312, 1.000000000000000000, 0.9510565162951535312, 1.000000000000000000, 0.9510565162951535312, 1.000000000000000000, 0.9755282581475777093, 0.9755282581475768211 ) ) 
 REPRESENTATION_ITEM ( '' )  );
#5524 = CARTESIAN_POINT ( 'NONE',  ( 47.43856463449117911, 109.7297705074273182, 35.64915139335015937 ) ) ;
#5525 = CARTESIAN_POINT ( 'NONE',  ( 17.60877916486148465, 96.95950790538488206, 1.267834678905774393 ) ) ;
#5526 = EDGE_LOOP ( 'NONE', ( #7904, #7670, #21323, #21268 ) ) ;
#5527 = CARTESIAN_POINT ( 'NONE',  ( 14.82803154953497859, 120.8649872489531987, 9.204245268424362081 ) ) ;
#5528 = ORIENTED_EDGE ( 'NONE', *, *, #20139, .T. ) ;
#5529 = VECTOR ( 'NONE', #18760, 1000.000000000000000 ) ;
#5530 = DIRECTION ( 'NONE',  ( 0.000000000000000000, -0.000000000000000000, 1.000000000000000000 ) ) ;
#5531 = CARTESIAN_POINT ( 'NONE',  ( 48.01140435219951996, 89.06049967264871725, 35.83527830041809636 ) ) ;
#5532 = CARTESIAN_POINT ( 'NONE',  ( 39.42975644700377558, 140.8151871740940067, 31.60846029578754468 ) ) ;
#5533 = CIRCLE ( 'NONE', #13986, 7.500000000000007105 ) ;
#5534 = CARTESIAN_POINT ( 'NONE',  ( 43.01140435219951286, 104.9604996726487514, 28.95336869806222779 ) ) ;
#5535 = CARTESIAN_POINT ( 'NONE',  ( 47.47886434171987702, 153.8471147930492862, -3.017879606865911502 ) ) ;
#5536 = CARTESIAN_POINT ( 'NONE',  ( 38.96631938032478359, 60.41049967264873288, 31.27175355779120025 ) ) ;
#5537 = EDGE_CURVE ( 'NONE', #11247, #32, #19298, .T. ) ;
#5538 = CARTESIAN_POINT ( 'NONE',  ( -151.4692556286852891, -169.7391397928655010, 60.17163382399899518 ) ) ;
#5539 = CARTESIAN_POINT ( 'NONE',  ( -159.5594255724347761, -181.8630981290893374, 43.77915905869157598 ) ) ;
#5540 = CARTESIAN_POINT ( 'NONE',  ( 47.05648932407426344, 63.98445800887257917, 37.14960608071593384 ) ) ;
#5541 = CARTESIAN_POINT ( 'NONE',  ( -159.5594255724347761, -163.2630981290893146, 55.53486410454104316 ) ) ;
#5542 = CARTESIAN_POINT ( 'NONE',  ( 45.74753988029933538, 85.42977050742730682, 37.97664729208901946 ) ) ;
#5543 = CARTESIAN_POINT ( 'NONE',  ( -159.0959885057557983, -161.1938272943107222, 44.11586579668791330 ) ) ;
#5544 = CARTESIAN_POINT ( 'NONE',  ( 43.01140435219951286, 83.36518717409398960, 29.55568802177586107 ) ) ;
#5545 = CARTESIAN_POINT ( 'NONE',  ( -88.69383338279318707, 132.1114735047150646, -35.00000000000000000 ) ) ;
#5546 = DIRECTION ( 'NONE',  ( -0.000000000000000000, 1.000000000000000000, -0.000000000000000000 ) ) ;
#5547 = ORIENTED_EDGE ( 'NONE', *, *, #1158, .T. ) ;
#5548 = CARTESIAN_POINT ( 'NONE',  ( 46.10157429594899270, 85.73445800887255075, 29.95742577749336988 ) ) ;
#5549 = DIRECTION ( 'NONE',  ( 0.000000000000000000, -0.000000000000000000, -1.000000000000000000 ) ) ;
#5550 = CARTESIAN_POINT ( 'NONE',  ( 44.37947211624943833, 131.4797705074273040, 30.00020018409699318 ) ) ;
#5551 = CARTESIAN_POINT ( 'NONE',  ( 70.48507635059884535, 125.9029633330538189, 6.422671151982867421 ) ) ;
#5552 = ORIENTED_EDGE ( 'NONE', *, *, #342, .F. ) ;
#5553 = VECTOR ( 'NONE', #18835, 1000.000000000000000 ) ;
#5554 = AXIS2_PLACEMENT_3D ( 'NONE', #4191, #20951, #1100 ) ;
#5555 = EDGE_CURVE ( 'NONE', #13376, #488, #6969, .T. ) ;
#5556 = CARTESIAN_POINT ( 'NONE',  ( 48.01140435219951996, 73.13445800887258486, 35.83527830041809636 ) ) ;
#5557 = ORIENTED_EDGE ( 'NONE', *, *, #8655, .F. ) ;
#5558 = CARTESIAN_POINT ( 'NONE',  ( 47.43856463449118621, 136.8797705074273381, 34.21067981925357060 ) ) ;
#5560 = EDGE_CURVE ( 'NONE', #10801, #6293, #557, .T. ) ;
#5559 = CARTESIAN_POINT ( 'NONE',  ( -149.8854112254399240, -180.3160212151857138, 39.65701158161629536 ) ) ;
#5561 = CYLINDRICAL_SURFACE ( 'NONE', #4129, 4.999999999999997335 ) ;
#5562 = CARTESIAN_POINT ( 'NONE',  ( 48.01140435219951996, 121.4344580088725820, 32.58608133808903773 ) ) ;
#5563 = CARTESIAN_POINT ( 'NONE',  ( 163.3401611601853745, 191.7221236944928364, 22.21121901686272793 ) ) ;
#5564 = EDGE_CURVE ( 'NONE', #11189, #19361, #15950, .T. ) ;
#5565 = CARTESIAN_POINT ( 'NONE',  ( 38.58424406990784661, 95.96518717409396970, 32.77220824515698183 ) ) ;
#5566 = CARTESIAN_POINT ( 'NONE',  ( -56.84366818088135176, 789.5005544000622422, -3.999999999999996447 ) ) ;
#5567 = CARTESIAN_POINT ( 'NONE',  ( 159.4819454078502190, 211.3876867681337046, 14.00000000000001776 ) ) ;
#5568 = CARTESIAN_POINT ( 'NONE',  ( -141.4692556286852891, -161.9130981290892919, 46.40781461928724383 ) ) ;
#5569 = CARTESIAN_POINT ( 'NONE',  ( 38.01140435219951996, 131.9344580088725820, 35.83527830041810347 ) ) ;
#5570 = CARTESIAN_POINT ( 'NONE',  ( 46.59305225739526435, 110.1797705074273210, 31.60846029578754468 ) ) ;
#5571 = CARTESIAN_POINT ( 'NONE',  ( 33.94330515458147346, 146.6952251797808628, -4.443226218224292978 ) ) ;
#5572 = CARTESIAN_POINT ( 'NONE',  ( -141.4692556286852891, -184.1391397928654783, 52.90620854394536821 ) ) ;
#5573 = CARTESIAN_POINT ( 'NONE',  ( 45.74753988029934249, 107.0651871740939782, 30.44471234641812174 ) ) ;
#5574 = VERTEX_POINT ( 'NONE', #19191 ) ;
#5575 = CARTESIAN_POINT ( 'NONE',  ( 47.05648932407426344, 76.58445800887257349, 31.27175355779120025 ) ) ;
#5576 = CARTESIAN_POINT ( 'NONE',  ( 23.17700876947760591, 147.8092992330439586, -3.851376987104358829 ) ) ;
#5577 = CARTESIAN_POINT ( 'NONE',  ( 34.07414013685151843, 93.16113583794900421, 7.775673839875955728 ) ) ;
#5578 = CARTESIAN_POINT ( 'NONE',  ( -148.3790856849358306, -169.5891397928654669, 59.16757674456786020 ) ) ;
#5579 = EDGE_CURVE ( 'NONE', #18715, #2680, #15868, .T. ) ;
#5580 = CARTESIAN_POINT ( 'NONE',  ( 39.42975644700377558, 78.67977050742732104, 36.81289934271958941 ) ) ;
#5581 = ORIENTED_EDGE ( 'NONE', *, *, #17717, .T. ) ;
#5582 = EDGE_CURVE ( 'NONE', #13398, #4862, #20344, .T. ) ;
#5583 =( BOUNDED_CURVE ( )  B_SPLINE_CURVE ( 2, ( #9808, #7931, #8043, #19495, #13103, #18282, #19716, #4717, #7722, #14854, #21376, #14636, #21600 ),
 .UNSPECIFIED., .F., .F. ) 
 B_SPLINE_CURVE_WITH_KNOTS ( ( 3, 2, 2, 2, 2, 2, 3 ),
 ( 0.5367647058823529216, 0.5382352941176470340, 0.5411764705882352589, 0.5441176470588234837, 0.5470588235294118196, 0.5500000000000000444, 0.5514705882352941568 ),
 .UNSPECIFIED. ) 
 CURVE ( )  GEOMETRIC_REPRESENTATION_ITEM ( )  RATIONAL_B_SPLINE_CURVE ( ( 0.9755282581475768211, 0.9755282581475768211, 1.000000000000000000, 0.9510565162951535312, 1.000000000000000000, 0.9510565162951535312, 1.000000000000000000, 0.9510565162951535312, 1.000000000000000000, 0.9510565162951535312, 1.000000000000000000, 0.9755282581475768211, 0.9755282581475768211 ) ) 
 REPRESENTATION_ITEM ( '' )  );
#5584 = CARTESIAN_POINT ( 'NONE',  ( 46.10157429594899270, 64.73445800887257917, 29.95742577749337343 ) ) ;
#5585 = CARTESIAN_POINT ( 'NONE',  ( -143.9637021292201950, -116.9891397928655010, 62.65701158161630957 ) ) ;
#5586 = CARTESIAN_POINT ( 'NONE',  ( 38.01140435219951996, 126.8604996726487144, 35.83527830041810347 ) ) ;
#5588 = CARTESIAN_POINT ( 'NONE',  ( 22.33864107606189719, 92.72021074822440312, 2.057911645927444244 ) ) ;
#5587 = CARTESIAN_POINT ( 'NONE',  ( 38.58424406990784661, 78.26518717409400949, 35.64915139335016647 ) ) ;
#5589 = CARTESIAN_POINT ( 'NONE',  ( -148.5561028927606344, -182.7938272943107449, 40.69124936498395328 ) ) ;
#5590 = DIRECTION ( 'NONE',  ( 0.000000000000000000, 0.000000000000000000, 1.000000000000000000 ) ) ;
#5591 = CARTESIAN_POINT ( 'NONE',  ( -157.6495955161842062, -188.0130981290892862, 41.15050349809590102 ) ) ;
#5592 = DIRECTION ( 'NONE',  ( 0.000000000000000000, -1.000000000000000000, 0.000000000000000000 ) ) ;
#5593 = CARTESIAN_POINT ( 'NONE',  ( -156.4692903108300186, -155.9898770414735623, 40.99677756761010272 ) ) ;
#5594 = CARTESIAN_POINT ( 'NONE',  ( 39.42975644700377558, 138.6797705074273210, 36.81289934271958941 ) ) ;
#5595 = CARTESIAN_POINT ( 'NONE',  ( 45.74753988029933538, 107.3297705074272983, 30.44471234641811819 ) ) ;
#5596 = CARTESIAN_POINT ( 'NONE',  ( 9.822352152143091431, 128.2981216602131553, 9.363167623699879982 ) ) ;
#5597 = CARTESIAN_POINT ( 'NONE',  ( 43.01140435219951286, 137.3651871740940180, 29.55568802177586107 ) ) ;
#5598 = VECTOR ( 'NONE', #16512, 1000.000000000000000 ) ;
#5599 = CARTESIAN_POINT ( 'NONE',  ( -154.3824083646099439, -155.4938272943107052, 40.69124936498395328 ) ) ;
#5600 = CARTESIAN_POINT ( 'NONE',  ( -142.0420953463935803, -165.5084106276440252, 46.59394152635518083 ) ) ;
#5601 = VECTOR ( 'NONE', #9019, 1000.000000000000000 ) ;
#5602 = CARTESIAN_POINT ( 'NONE',  ( -151.4692556286852891, -196.9891397928655010, 49.65701158161630957 ) ) ;
#5603 = CARTESIAN_POINT ( 'NONE',  ( 42.21948215057684450, 136.3836182503284533, 39.21067981925355639 ) ) ;
#5604 = CARTESIAN_POINT ( 'NONE',  ( 19.04663372520828801, 134.9227921665808765, 15.79488502079956547 ) ) ;
#5605 = DIRECTION ( 'NONE',  ( 0.000000000000000000, -1.000000000000000000, 0.000000000000000000 ) ) ;
#5606 = CARTESIAN_POINT ( 'NONE',  ( 47.43856463449117200, 112.7651871740940095, 32.77220824515698183 ) ) ;
#5607 = EDGE_CURVE ( 'NONE', #1905, #21813, #3877, .T. ) ;
#5608 = EDGE_CURVE ( 'NONE', #19825, #12794, #4136, .T. ) ;
#5609 = VERTEX_POINT ( 'NONE', #14108 ) ;
#5610 = CARTESIAN_POINT ( 'NONE',  ( 138.4989748031516967, 208.9305787985672680, -44.99999999999997158 ) ) ;
#5611 = ORIENTED_EDGE ( 'NONE', *, *, #15022, .F. ) ;
#5612 = CARTESIAN_POINT ( 'NONE',  ( 39.92123440845004723, 90.23445800887257917, 38.46393386101376421 ) ) ;
#5613 = CARTESIAN_POINT ( 'NONE',  ( 43.01140435219951286, 146.6297705074273097, 29.55568802177586107 ) ) ;
#5614 = APPLICATION_CONTEXT ( 'automotive_design' ) ;
#5615 =( GEOMETRIC_REPRESENTATION_CONTEXT ( 3 ) GLOBAL_UNCERTAINTY_ASSIGNED_CONTEXT ( ( #3361 ) ) GLOBAL_UNIT_ASSIGNED_CONTEXT ( ( #1045, #1369, #18113 ) ) REPRESENTATION_CONTEXT ( 'NONE', 'WORKASPACE' ) );
#5616 = CARTESIAN_POINT ( 'NONE',  ( 43.01140435219951286, 61.12977050742731677, 38.86567161673127657 ) ) ;
#5618 = CARTESIAN_POINT ( 'NONE',  ( 39.35338560254503903, 91.94623120232463975, 14.56122079753911081 ) ) ;
#5617 = CARTESIAN_POINT ( 'NONE',  ( 38.58424406990784661, 114.2651871740940095, 35.64915139335016647 ) ) ;
#5619 = CARTESIAN_POINT ( 'NONE',  ( 38.01140435219952707, 72.71049967264873715, 34.21067981925357060 ) ) ;
#5620 = EDGE_CURVE ( 'NONE', #1584, #19429, #12028, .T. ) ;
#5622 = CARTESIAN_POINT ( 'NONE',  ( 43.01140435219951286, 75.53445800887257633, 39.21067981925356349 ) ) ;
#5621 = CARTESIAN_POINT ( 'NONE',  ( 43.01140435219951286, 77.03445800887257633, 29.21067981925356705 ) ) ;
#5623 = CARTESIAN_POINT ( 'NONE',  ( 0.000000000000000000, 0.000000000000000000, -44.99999999999997158 ) ) ;
#5624 = CARTESIAN_POINT ( 'NONE',  ( 38.96631938032478359, 72.08445800887257349, 37.14960608071593384 ) ) ;
#5625 = CARTESIAN_POINT ( 'NONE',  ( 40.27526882409969033, 72.56518717409399244, 37.97664729208901946 ) ) ;
#5626 = CARTESIAN_POINT ( 'NONE',  ( 42.21948215057684450, 63.03738109496900677, 29.21067981925356705 ) ) ;
#5627 = CARTESIAN_POINT ( 'NONE',  ( -160.8964159109769696, -182.0438272943107449, 46.59394152635518793 ) ) ;
#5628 = DIRECTION ( 'NONE',  ( 1.000000000000000000, 0.000000000000000000, 0.000000000000000000 ) ) ;
#5629 = VERTEX_POINT ( 'NONE', #2538 ) ;
#5630 = CARTESIAN_POINT ( 'NONE',  ( 36.32848368193762667, 153.5644447507555981, 2.620555573812929584 ) ) ;
#5631 = ADVANCED_FACE ( 'NONE', ( #8948 ), #15655, .F. ) ;
#5632 = ORIENTED_EDGE ( 'NONE', *, *, #6281, .T. ) ;
#5633 = CARTESIAN_POINT ( 'NONE',  ( 40.27526882409969033, 147.5651871740939498, 37.97664729208901946 ) ) ;
#5634 = AXIS2_PLACEMENT_3D ( 'NONE', #3751, #12113, #15102 ) ;
#5635 = AXIS2_PLACEMENT_3D ( 'NONE', #2058, #5680, #7244 ) ;
#5636 = DIRECTION ( 'NONE',  ( 0.000000000000000000, 0.000000000000000000, 1.000000000000000000 ) ) ;
#5637 = CARTESIAN_POINT ( 'NONE',  ( 41.64333658814960870, 107.7797705074273154, 30.00020018409699318 ) ) ;
#5638 = ORIENTED_EDGE ( 'NONE', *, *, #5672, .T. ) ;
#5639 = ORIENTED_EDGE ( 'NONE', *, *, #12879, .T. ) ;
#5640 = CARTESIAN_POINT ( 'NONE',  ( 67.71458430423905384, 106.3058120325361671, 6.227933542621733487 ) ) ;
#5641 = ORIENTED_EDGE ( 'NONE', *, *, #21598, .T. ) ;
#5642 = CARTESIAN_POINT ( 'NONE',  ( 45.74753988029933538, 112.4297705074273210, 37.97664729208901946 ) ) ;
#5643 = EDGE_CURVE ( 'NONE', #15461, #6487, #672, .T. ) ;
#5644 = CARTESIAN_POINT ( 'NONE',  ( 48.01140435219951996, 89.21049967264873715, 34.21067981925357060 ) ) ;
#5645 = CARTESIAN_POINT ( 'NONE',  ( 47.43856463449118621, 82.87977050742730967, 34.21067981925357060 ) ) ;
#5646 = CARTESIAN_POINT ( 'NONE',  ( 45.74753988029933538, 145.1651871740939725, 37.97664729208901946 ) ) ;
#5647 = CARTESIAN_POINT ( 'NONE',  ( 39.92123440845004723, 102.2604996726487201, 29.95742577749337343 ) ) ;
#5648 = CARTESIAN_POINT ( 'NONE',  ( 10.42839491720816625, 130.4056617841633283, -4.565575592310756825 ) ) ;
#5649 = CIRCLE ( 'NONE', #17965, 7.500000000000000000 ) ;
#5650 = CYLINDRICAL_SURFACE ( 'NONE', #17032, 10.00000000000000888 ) ;
#5651 = CARTESIAN_POINT ( 'NONE',  ( 136.0451547902032701, 182.4218825594992950, 19.19853326693791473 ) ) ;
#5652 = CARTESIAN_POINT ( 'NONE',  ( -143.3790856849358306, -174.6891397928654612, 43.77915905869157598 ) ) ;
#5653 = DIRECTION ( 'NONE',  ( 1.000000000000000000, 0.000000000000000000, 0.000000000000000000 ) ) ;
#5654 = CARTESIAN_POINT ( 'NONE',  ( 39.92123440845005433, 143.3344580088725877, 29.95742577749336988 ) ) ;
#5655 = LINE ( 'NONE', #9085, #6403 ) ;
#5656 = ORIENTED_EDGE ( 'NONE', *, *, #11935, .T. ) ;
#5657 = CARTESIAN_POINT ( 'NONE',  ( 44.37947211624943833, 82.27977050742732956, 38.42115945441014446 ) ) ;
#5658 = CARTESIAN_POINT ( 'NONE',  ( -145.6429501568359797, -164.9438272943106938, 41.63779006702063867 ) ) ;
#5659 = CARTESIAN_POINT ( 'NONE',  ( 45.74753988029934249, 82.16518717409400097, 37.97664729208901235 ) ) ;
#5660 = CARTESIAN_POINT ( 'NONE',  ( 76.79083979644461522, 114.3551126354810492, -1.232281421064668869 ) ) ;
#5661 = CARTESIAN_POINT ( 'NONE',  ( -160.8964159109769696, -194.1584106276440593, 49.65701158161630957 ) ) ;
#5662 = VERTEX_POINT ( 'NONE', #10496 ) ;
#5663 = CARTESIAN_POINT ( 'NONE',  ( -151.4692556286853176, -174.8130981290893260, 59.65701158161632378 ) ) ;
#5664 = LINE ( 'NONE', #13929, #16586 ) ;
#5665 = CARTESIAN_POINT ( 'NONE',  ( 39.42975644700377558, 135.0797705074272983, 31.60846029578754468 ) ) ;
#5666 = CARTESIAN_POINT ( 'NONE',  ( 69.68093098098093208, 128.8215514297462789, 6.303499042945750475 ) ) ;
#5667 = VERTEX_POINT ( 'NONE', #15554 ) ;
#5668 = CYLINDRICAL_SURFACE ( 'NONE', #8344, 10.00000000000000888 ) ;
#5669 = EDGE_CURVE ( 'NONE', #8397, #19825, #457, .T. ) ;
#5670 = ORIENTED_EDGE ( 'NONE', *, *, #8655, .T. ) ;
#5671 = CARTESIAN_POINT ( 'NONE',  ( 39.42975644700377558, 138.6797705074273210, 36.81289934271958941 ) ) ;
#5672 = EDGE_CURVE ( 'NONE', #19018, #15353, #18211, .T. ) ;
#5673 = FACE_OUTER_BOUND ( 'NONE', #15781, .T. ) ;
#5674 = CARTESIAN_POINT ( 'NONE',  ( 48.01140435219951996, 121.1344580088725706, 35.83527830041809636 ) ) ;
#5675 = EDGE_CURVE ( 'NONE', #6431, #7690, #1479, .T. ) ;
#5676 = CARTESIAN_POINT ( 'NONE',  ( 38.58424406990784661, 92.96518717409401233, 32.77220824515698183 ) ) ;
#5677 = CARTESIAN_POINT ( 'NONE',  ( 43.80332655382220253, 74.88361825032848174, 29.21067981925356705 ) ) ;
#5678 = CARTESIAN_POINT ( 'NONE',  ( -151.4692556286852891, -126.9891397928655010, 49.65701158161630957 ) ) ;
#5679 = CARTESIAN_POINT ( 'NONE',  ( -145.2889157411863721, -156.5130981290892862, 58.16351966513671812 ) ) ;
#5680 = DIRECTION ( 'NONE',  ( 0.000000000000000000, 0.000000000000000000, 1.000000000000000000 ) ) ;
#5681 = CARTESIAN_POINT ( 'NONE',  ( 43.01140435219954838, 108.5344580088725763, 39.21067981925356349 ) ) ;
#5682 = CARTESIAN_POINT ( 'NONE',  ( 38.96631938032478359, 137.4844580088725650, 31.27175355779120025 ) ) ;
#5683 = CARTESIAN_POINT ( 'NONE',  ( 41.64333658814960870, 111.9797705074273324, 38.42115945441014446 ) ) ;
#5684 = ADVANCED_FACE ( 'NONE', ( #14543 ), #5046, .F. ) ;
#5685 = CARTESIAN_POINT ( 'NONE',  ( 37.19530960600651071, 92.23011878076297876, 13.65210914576621271 ) ) ;
#5686 = CARTESIAN_POINT ( 'NONE',  ( -154.3824083646099439, -190.2938272943107449, 58.62277379824867296 ) ) ;
#5687 = CARTESIAN_POINT ( 'NONE',  ( 43.01140435219951286, 104.3651871740940038, 29.55568802177586107 ) ) ;
#5688 = FACE_OUTER_BOUND ( 'NONE', #12938, .T. ) ;
#5689 = EDGE_LOOP ( 'NONE', ( #15384, #14421, #8334, #5639, #2466, #13181 ) ) ;
#5690 = CARTESIAN_POINT ( 'NONE',  ( 43.01140435219951286, 86.96049967264872294, 29.21067981925356705 ) ) ;
#5691 = CARTESIAN_POINT ( 'NONE',  ( 18.35401747797491723, 143.4883766228698221, 10.92869415326320670 ) ) ;
#5692 = CARTESIAN_POINT ( 'NONE',  ( 17.98614708603287937, 106.9092867359673704, 15.63253669370310384 ) ) ;
#5693 = DIRECTION ( 'NONE',  ( 0.000000000000000000, 1.000000000000000000, 0.000000000000000000 ) ) ;
#5694 = CIRCLE ( 'NONE', #19426, 2.999999999999997780 ) ;
#5695 = CIRCLE ( 'NONE', #17315, 24.99999999999999289 ) ;
#5696 = CARTESIAN_POINT ( 'NONE',  ( 47.43856463449117911, 79.72977050742730398, 35.64915139335015937 ) ) ;
#5697 = ORIENTED_EDGE ( 'NONE', *, *, #11604, .T. ) ;
#5698 = VERTEX_POINT ( 'NONE', #12788 ) ;
#5699 = CARTESIAN_POINT ( 'NONE',  ( 43.01140435219951286, 65.03445800887257633, 28.95336869806222779 ) ) ;
#5700 = PLANE ( 'NONE',  #21103 ) ;
#5701 = CARTESIAN_POINT ( 'NONE',  ( 47.05648932407426344, 116.5104996726487485, 31.27175355779120025 ) ) ;
#5703 = CARTESIAN_POINT ( 'NONE',  ( 29.26409511065843105, 88.64202804534433255, -5.203872050689020590 ) ) ;
#5702 = CARTESIAN_POINT ( 'NONE',  ( 39.42975644700377558, 77.81518717409399244, 31.60846029578754468 ) ) ;
#5704 = CARTESIAN_POINT ( 'NONE',  ( -159.0959885057557983, -182.1938272943107506, 44.11586579668791330 ) ) ;
#5705 = CARTESIAN_POINT ( 'NONE',  ( 76.40658810299491677, 127.4365358892444959, 12.33923360994393903 ) ) ;
#5706 = CARTESIAN_POINT ( 'NONE',  ( -141.4692556286852891, -189.0630981290892976, 49.65701158161630957 ) ) ;
#5707 = PRESENTATION_LAYER_ASSIGNMENT (  '', '', ( #10302 ) ) ;
#5708 = DIRECTION ( 'NONE',  ( -0.000000000000000000, -0.000000000000000000, 1.000000000000000000 ) ) ;
#5709 = CARTESIAN_POINT ( 'NONE',  ( -156.1828648351502409, -155.3945647575687872, 41.49286807254280518 ) ) ;
#5710 = CARTESIAN_POINT ( 'NONE',  ( 45.74753988029933538, 140.3297705074272983, 30.44471234641811819 ) ) ;
#5711 = CARTESIAN_POINT ( 'NONE',  ( 75.25890017065090376, 108.1762305904371004, -2.022566849933696620 ) ) ;
#5712 = CARTESIAN_POINT ( 'NONE',  ( 39.42975644700377558, 131.8151871740940067, 31.60846029578754468 ) ) ;
#5713 = CARTESIAN_POINT ( 'NONE',  ( 48.01140435219951996, 67.43445800887256780, 32.58608133808903773 ) ) ;
#5714 = CARTESIAN_POINT ( 'NONE',  ( -159.0959885057557983, -167.4584106276440423, 44.11586579668791330 ) ) ;
#5715 = CARTESIAN_POINT ( 'NONE',  ( 38.58424406990784661, 60.52977050742731535, 35.64915139335016647 ) ) ;
#5716 = FACE_BOUND ( 'NONE', #17871, .T. ) ;
#5717 = EDGE_CURVE ( 'NONE', #9069, #5138, #2861, .T. ) ;
#5718 = CARTESIAN_POINT ( 'NONE',  ( 16.98434641657835797, 108.8433182140206270, 14.72356627441054755 ) ) ;
#5719 = CARTESIAN_POINT ( 'NONE',  ( 43.01140435219953417, 142.4604996726487514, 39.21067981925356349 ) ) ;
#5720 = CARTESIAN_POINT ( 'NONE',  ( 47.43856463449117200, 118.4651871740939981, 35.64915139335016647 ) ) ;
#5721 =( BOUNDED_CURVE ( )  B_SPLINE_CURVE ( 2, ( #13002, #14754, #9920, #19834, #16735, #11336, #3191, #3077, #11560, #21607, #18288, #18058, #8050 ),
 .UNSPECIFIED., .F., .F. ) 
 B_SPLINE_CURVE_WITH_KNOTS ( ( 3, 2, 2, 2, 2, 2, 3 ),
 ( 0.3750000000000000000, 0.3785714285714285587, 0.3857142857142857317, 0.3928571428571428492, 0.4000000000000000222, 0.4071428571428571397, 0.4107142857142857539 ),
 .UNSPECIFIED. ) 
 CURVE ( )  GEOMETRIC_REPRESENTATION_ITEM ( )  RATIONAL_B_SPLINE_CURVE ( ( 0.9755282581475768211, 0.9755282581475768211, 1.000000000000000000, 0.9510565162951535312, 1.000000000000000000, 0.9510565162951535312, 1.000000000000000000, 0.9510565162951535312, 1.000000000000000000, 0.9510565162951535312, 1.000000000000000000, 0.9755282581475765991, 0.9755282581475768211 ) ) 
 REPRESENTATION_ITEM ( '' )  );
#5722 = ORIENTED_EDGE ( 'NONE', *, *, #6927, .T. ) ;
#5723 = DIRECTION ( 'NONE',  ( 2.779543948608941985E-16, -1.000000000000000000, 0.000000000000000000 ) ) ;
#5724 = VERTEX_POINT ( 'NONE', #14328 ) ;
#5725 = CARTESIAN_POINT ( 'NONE',  ( 47.05648932407426344, 87.98445800887257917, 37.14960608071593384 ) ) ;
#5726 = CARTESIAN_POINT ( 'NONE',  ( 47.43856463449117911, 149.0297705074273154, 32.77220824515697473 ) ) ;
#5727 = CARTESIAN_POINT ( 'NONE',  ( 47.05648932407426344, 149.5104996726487343, 31.27175355779120025 ) ) ;
#5729 = CARTESIAN_POINT ( 'NONE',  ( 38.46765184765857981, 147.6574975633170936, -2.267929528491105629 ) ) ;
#5728 = CARTESIAN_POINT ( 'NONE',  ( 46.59305225739526435, 103.3151871740940067, 36.81289934271958941 ) ) ;
#5730 = CARTESIAN_POINT ( 'NONE',  ( 41.46631938032478359, 75.11049967264874283, 29.45539723777780239 ) ) ;
#5732 = DIRECTION ( 'NONE',  ( 1.000000000000000000, 0.000000000000000000, 0.000000000000000000 ) ) ;
#5731 = CARTESIAN_POINT ( 'NONE',  ( 43.01140435219954838, 108.5344580088725763, 39.21067981925356349 ) ) ;
#5733 = EDGE_CURVE ( 'NONE', #4745, #14655, #3280, .T. ) ;
#5734 = ADVANCED_FACE ( 'NONE', ( #16303 ), #8356, .T. ) ;
#5735 = CARTESIAN_POINT ( 'NONE',  ( -161.4692556286852891, -172.4130981290892919, 52.90620854394536821 ) ) ;
#5736 = DIRECTION ( 'NONE',  ( 1.000000000000000000, 0.000000000000000000, -1.734723475976805615E-16 ) ) ;
#5737 = CARTESIAN_POINT ( 'NONE',  ( -81.10645082872859746, 10.96617311717548837, 4.000000000000021316 ) ) ;
#5738 = CARTESIAN_POINT ( 'NONE',  ( -142.0420953463936087, -177.3938272943107393, 49.65701158161630957 ) ) ;
#5739 = CARTESIAN_POINT ( 'NONE',  ( -157.2955611005345986, -194.6084106276440195, 41.63779006702063867 ) ) ;
#5740 = EDGE_LOOP ( 'NONE', ( #11373, #10373 ) ) ;
#5741 = CARTESIAN_POINT ( 'NONE',  ( 75.01029411920679024, 107.5147569559006655, 5.001370044594233732 ) ) ;
#5742 = DIRECTION ( 'NONE',  ( -0.000000000000000000, 1.000000000000000000, -0.000000000000000000 ) ) ;
#5743 = CARTESIAN_POINT ( 'NONE',  ( 41.64333658814960870, 140.5151871740939953, 30.00020018409699318 ) ) ;
#5744 = CARTESIAN_POINT ( 'NONE',  ( 38.58424406990785371, 155.9651871740939555, 32.77220824515697473 ) ) ;
#5745 = CARTESIAN_POINT ( 'NONE',  ( 43.01140435219951286, 107.6297705074273097, 29.55568802177586107 ) ) ;
#5746 = ORIENTED_EDGE ( 'NONE', *, *, #9783, .T. ) ;
#5747 = ORIENTED_EDGE ( 'NONE', *, *, #10121, .F. ) ;
#5748 = CARTESIAN_POINT ( 'NONE',  ( 21.71662816054514167, 101.4213758857254675, 8.370706496969875232 ) ) ;
#5749 = ORIENTED_EDGE ( 'NONE', *, *, #15830, .T. ) ;
#5750 = CARTESIAN_POINT ( 'NONE',  ( 173.3794444120442222, -37.13255853780189852, 19.99999999999999645 ) ) ;
#5751 = CARTESIAN_POINT ( 'NONE',  ( 47.43856463449117200, 133.7651871740939669, 32.77220824515698183 ) ) ;
#5752 = CARTESIAN_POINT ( 'NONE',  ( 38.01140435219951996, 105.8604996726487570, 35.83527830041810347 ) ) ;
#5753 = CARTESIAN_POINT ( 'NONE',  ( 26.13368487350976110, 90.12329638092472806, 0.9106621812756837686 ) ) ;
#5754 = ADVANCED_FACE ( 'NONE', ( #7946 ), #14652, .T. ) ;
#5755 = CARTESIAN_POINT ( 'NONE',  ( 136.1510593568410172, 182.1483534088744420, 19.85643285628697541 ) ) ;
#5756 = CARTESIAN_POINT ( 'NONE',  ( -154.5594255724347761, -171.0891397928654669, 40.14644641866476604 ) ) ;
#5757 = CARTESIAN_POINT ( 'NONE',  ( 44.55648932407425633, 158.8104996726487457, 29.45539723777780239 ) ) ;
#5758 = UNCERTAINTY_MEASURE_WITH_UNIT (LENGTH_MEASURE( 1.000000000000000082E-05 ), #9575, 'distance_accuracy_value', 'NONE');
#5759 = DIRECTION ( 'NONE',  ( 0.000000000000000000, 1.000000000000000000, 0.000000000000000000 ) ) ;
#5760 = CARTESIAN_POINT ( 'NONE',  ( -120.0322075325610598, -126.9891397928655010, -34.99999999999999289 ) ) ;
#5761 = VERTEX_POINT ( 'NONE', #21069 ) ;
#5762 = CARTESIAN_POINT ( 'NONE',  ( 38.58424406990784661, 87.22977050742731819, 32.77220824515698183 ) ) ;
#5763 = CARTESIAN_POINT ( 'NONE',  ( -160.8964159109769696, -163.8938272943107393, 49.65701158161630957 ) ) ;
#5764 = CARTESIAN_POINT ( 'NONE',  ( 39.42975644700377558, 66.41518717409400097, 36.81289934271958941 ) ) ;
#5765 = CARTESIAN_POINT ( 'NONE',  ( 71.86557814238962294, 101.4853659568252766, -7.779689512009451136 ) ) ;
#5766 = CARTESIAN_POINT ( 'NONE',  ( -145.6429501568359797, -192.2084106276440139, 41.63779006702063867 ) ) ;
#5767 = ORIENTED_EDGE ( 'NONE', *, *, #20576, .T. ) ;
#5768 = CARTESIAN_POINT ( 'NONE',  ( 48.01140435219951996, 85.43445800887255359, 32.58608133808903773 ) ) ;
#5769 = CARTESIAN_POINT ( 'NONE',  ( 42.21948215057684450, 104.1113394311928460, 29.21067981925356705 ) ) ;
#5770 = CARTESIAN_POINT ( 'NONE',  ( 44.37947211624943833, 137.4797705074273324, 30.00020018409699318 ) ) ;
#5771 = CARTESIAN_POINT ( 'NONE',  ( 29.11053999216420252, 151.1052802516552163, -16.63225393015772724 ) ) ;
#5772 = ORIENTED_EDGE ( 'NONE', *, *, #19850, .T. ) ;
#5773 = CARTESIAN_POINT ( 'NONE',  ( 174.0518276614676267, 207.1825338655619646, 21.73429951086134082 ) ) ;
#5774 = ORIENTED_EDGE ( 'NONE', *, *, #12879, .F. ) ;
#5775 = CARTESIAN_POINT ( 'NONE',  ( 38.58424406990784661, 123.5297705074273438, 35.64915139335016647 ) ) ;
#5776 = CARTESIAN_POINT ( 'NONE',  ( 42.21948215057684450, 111.4575765865523067, 39.21067981925355639 ) ) ;
#5777 = DIRECTION ( 'NONE',  ( -0.000000000000000000, -0.000000000000000000, 1.000000000000000000 ) ) ;
#5778 = CARTESIAN_POINT ( 'NONE',  ( -145.2889157411863437, -192.5130981290892862, 58.16351966513671812 ) ) ;
#5779 = CIRCLE ( 'NONE', #7222, 10.00000000000000888 ) ;
#5780 = CARTESIAN_POINT ( 'NONE',  ( 47.43856463449118621, 97.61518717409400381, 34.21067981925357060 ) ) ;
#5781 = DIRECTION ( 'NONE',  ( -0.000000000000000000, -0.000000000000000000, 1.000000000000000000 ) ) ;
#5782 = DIRECTION ( 'NONE',  ( 1.000000000000000000, 0.000000000000000000, 0.000000000000000000 ) ) ;
#5783 = CARTESIAN_POINT ( 'NONE',  ( -143.3790856849358306, -159.3630981290893089, 55.53486410454105027 ) ) ;
#5784 = PRODUCT_CONTEXT ( 'NONE', #7051, 'mechanical' ) ;
#5785 = CARTESIAN_POINT ( 'NONE',  ( 42.21948215057684450, 132.4575765865522783, 39.21067981925356349 ) ) ;
#5786 = CARTESIAN_POINT ( 'NONE',  ( 47.05648932407426344, 133.5844580088725877, 31.27175355779120025 ) ) ;
#5787 = CARTESIAN_POINT ( 'NONE',  ( 45.74753988029933538, 118.4297705074272926, 37.97664729208901946 ) ) ;
#5788 = CARTESIAN_POINT ( 'NONE',  ( 22.35924357203464297, 139.2281224154095014, 9.009280560090923373 ) ) ;
#5789 = CARTESIAN_POINT ( 'NONE',  ( 43.01140435219951996, 10.71049967264875491, 34.21067981925357060 ) ) ;
#5790 = CARTESIAN_POINT ( 'NONE',  ( 43.01140435219951286, 98.36518717409400381, 29.55568802177586107 ) ) ;
#5791 = DIRECTION ( 'NONE',  ( 0.000000000000000000, 0.000000000000000000, 1.000000000000000000 ) ) ;
#5792 = ORIENTED_EDGE ( 'NONE', *, *, #1857, .F. ) ;
#5793 = CARTESIAN_POINT ( 'NONE',  ( 43.80332655382220253, 75.61133943119284595, 39.21067981925355639 ) ) ;
#5794 = CARTESIAN_POINT ( 'NONE',  ( 71.86557814238962294, 101.4853659568252766, -7.779689512009451136 ) ) ;
#5795 = CARTESIAN_POINT ( 'NONE',  ( 70.74141321743030630, 114.7826485538520416, 5.870819564965037429 ) ) ;
#5796 = CYLINDRICAL_SURFACE ( 'NONE', #182, 4.999999999999997335 ) ;
#5797 = CARTESIAN_POINT ( 'NONE',  ( 38.58424406990786082, 81.37977050742730967, 34.21067981925357060 ) ) ;
#5798 = ORIENTED_EDGE ( 'NONE', *, *, #21582, .T. ) ;
#5799 = ORIENTED_EDGE ( 'NONE', *, *, #11278, .F. ) ;
#5800 = CARTESIAN_POINT ( 'NONE',  ( 18.67254549292281141, -61.68114226949890622, 20.00000000000000355 ) ) ;
#5801 = AXIS2_PLACEMENT_3D ( 'NONE', #20467, #18807, #10442 ) ;
#5802 = CARTESIAN_POINT ( 'NONE',  ( 43.01140435219951286, 121.4604996726487514, 39.46799094044489209 ) ) ;
#5804 = CARTESIAN_POINT ( 'NONE',  ( 11.65896226128411683, 106.3627486108568547, -4.370744638174604013 ) ) ;
#5803 = CARTESIAN_POINT ( 'NONE',  ( 43.01140435219951286, 80.36518717409398960, 29.55568802177586463 ) ) ;
#5805 = CARTESIAN_POINT ( 'NONE',  ( -160.8964159109769696, -166.8938272943107393, 49.65701158161630957 ) ) ;
#5806 = CARTESIAN_POINT ( 'NONE',  ( 45.29500579500201951, 154.0643053174194961, 10.91066218119221709 ) ) ;
#5807 = CARTESIAN_POINT ( 'NONE',  ( -151.4692556286852891, -185.3130981290893260, 39.14238933923362396 ) ) ;
#5808 = CARTESIAN_POINT ( 'NONE',  ( -176.9699209214867608, 160.7104996726487514, -35.00000000000000000 ) ) ;
#5810 = EDGE_CURVE ( 'NONE', #1249, #19734, #14847, .T. ) ;
#5809 = CARTESIAN_POINT ( 'NONE',  ( 156.7804311855217065, 208.8003142469820830, -44.99999999999997158 ) ) ;
#5811 = CARTESIAN_POINT ( 'NONE',  ( 44.37947211624943833, 139.2797705074273154, 38.42115945441014446 ) ) ;
#5812 = CARTESIAN_POINT ( 'NONE',  ( 76.33227852969314142, 111.7084249013780806, -2.141487123205697340 ) ) ;
#5813 = CARTESIAN_POINT ( 'NONE',  ( 43.01140435219951286, 129.8651871740940180, 38.86567161673127657 ) ) ;
#5814 = CARTESIAN_POINT ( 'NONE',  ( 46.10157429594899270, 137.6604996726487400, 29.95742577749336988 ) ) ;
#5815 = CARTESIAN_POINT ( 'NONE',  ( -145.6429501568359797, -165.2084106276440139, 41.63779006702063867 ) ) ;
#5816 = CARTESIAN_POINT ( 'NONE',  ( 43.01140435219951286, 79.46049967264875136, 39.21067981925356349 ) ) ;
#5817 = DIRECTION ( 'NONE',  ( -0.000000000000000000, 1.000000000000000000, -0.000000000000000000 ) ) ;
#5818 = CARTESIAN_POINT ( 'NONE',  ( 29.27693512915957541, 95.18479568265063051, 6.985315079919499404 ) ) ;
#5819 = CIRCLE ( 'NONE', #1266, 15.54735917280169311 ) ;
#5820 = DIRECTION ( 'NONE',  ( 0.000000000000000000, 0.000000000000000000, 1.000000000000000000 ) ) ;
#5821 = CARTESIAN_POINT ( 'NONE',  ( 47.43856463449117200, 106.7651871740939811, 32.77220824515698183 ) ) ;
#5822 = ORIENTED_EDGE ( 'NONE', *, *, #1202, .T. ) ;
#5823 = ADVANCED_FACE ( 'NONE', ( #12678 ), #4624, .F. ) ;
#5824 = LINE ( 'NONE', #7174, #20157 ) ;
#5825 = ORIENTED_EDGE ( 'NONE', *, *, #18959, .T. ) ;
#5826 = CARTESIAN_POINT ( 'NONE',  ( 41.46631938032478359, 95.18445800887258201, 29.45539723777780239 ) ) ;
#5827 = CARTESIAN_POINT ( 'NONE',  ( 38.01140435219952707, 144.7104996726487229, 34.21067981925357060 ) ) ;
#5829 = CARTESIAN_POINT ( 'NONE',  ( 46.87248680087107999, 147.7605717807558676, -8.934501345478663481 ) ) ;
#5828 = CARTESIAN_POINT ( 'NONE',  ( 47.43856463449117200, 109.7651871740939953, 32.77220824515698183 ) ) ;
#5830 = EDGE_CURVE ( 'NONE', #17591, #8610, #16715, .T. ) ;
#5831 = CARTESIAN_POINT ( 'NONE',  ( 44.55648932407425633, 61.61049967264874283, 38.96596240072933170 ) ) ;
#5833 = CARTESIAN_POINT ( 'NONE',  ( 163.1026836591718734, 192.4288937294299160, 18.98992973508700643 ) ) ;
#5832 = DIRECTION ( 'NONE',  ( -0.000000000000000000, -0.000000000000000000, -1.000000000000000000 ) ) ;
#5834 = CARTESIAN_POINT ( 'NONE',  ( 44.55648932407425633, 117.6844580088725820, 38.96596240072933170 ) ) ;
#5835 = AXIS2_PLACEMENT_3D ( 'NONE', #10467, #3844, #17167 ) ;
#5836 = CARTESIAN_POINT ( 'NONE',  ( -157.6495955161842062, -188.0130981290892862, 41.15050349809589392 ) ) ;
#5837 = DIRECTION ( 'NONE',  ( -0.000000000000000000, 1.000000000000000000, -0.000000000000000000 ) ) ;
#5838 = CARTESIAN_POINT ( 'NONE',  ( 38.58424406990784661, 65.96518717409399812, 32.77220824515698183 ) ) ;
#5839 = CARTESIAN_POINT ( 'NONE',  ( 77.15313604554262383, 122.4041478163663612, -8.494263314424808087 ) ) ;
#5840 = ADVANCED_FACE ( 'NONE', ( #20366 ), #18813, .F. ) ;
#5841 = DIRECTION ( 'NONE',  ( 1.000000000000000000, 0.000000000000000000, -1.734723475976805615E-16 ) ) ;
#5842 = CARTESIAN_POINT ( 'NONE',  ( -159.0959885057557983, -169.5938272943107279, 55.19815736654470584 ) ) ;
#5843 = CYLINDRICAL_SURFACE ( 'NONE', #4636, 10.00000000000000888 ) ;
#5844 = ORIENTED_EDGE ( 'NONE', *, *, #1697, .T. ) ;
#5845 =( BOUNDED_CURVE ( )  B_SPLINE_CURVE ( 2, ( #6042, #16068, #11324, #9480, #2521, #4182, #4384, #6146, #14420, #981, #12993, #21485, #7719 ),
 .UNSPECIFIED., .F., .F. ) 
 B_SPLINE_CURVE_WITH_KNOTS ( ( 3, 2, 2, 2, 2, 2, 3 ),
 ( 0.9107142857142856984, 0.9142857142857142572, 0.9214285714285713746, 0.9285714285714286031, 0.9357142857142857206, 0.9428571428571428381, 0.9464285714285713969 ),
 .UNSPECIFIED. ) 
 CURVE ( )  GEOMETRIC_REPRESENTATION_ITEM ( )  RATIONAL_B_SPLINE_CURVE ( ( 0.9755282581475768211, 0.9755282581475768211, 1.000000000000000000, 0.9510565162951535312, 1.000000000000000000, 0.9510565162951535312, 1.000000000000000000, 0.9510565162951535312, 1.000000000000000000, 0.9510565162951535312, 1.000000000000000000, 0.9755282581475768211, 0.9755282581475768211 ) ) 
 REPRESENTATION_ITEM ( '' )  );
#5846 = CARTESIAN_POINT ( 'NONE',  ( -154.3824083646099439, -179.7584106276440536, 40.69124936498395328 ) ) ;
#5847 = CARTESIAN_POINT ( 'NONE',  ( 13.73412108254838238, 102.0109333093626134, 0.4776103675054816922 ) ) ;
#5848 = VERTEX_POINT ( 'NONE', #13627 ) ;
#5849 = CARTESIAN_POINT ( 'NONE',  ( 45.74753988029933538, 145.1651871740939725, 37.97664729208901946 ) ) ;
#5850 = CARTESIAN_POINT ( 'NONE',  ( 41.64333658814960870, 93.97977050742733240, 38.42115945441014446 ) ) ;
#5851 = ORIENTED_EDGE ( 'NONE', *, *, #490, .F. ) ;
#5852 = ORIENTED_EDGE ( 'NONE', *, *, #2850, .T. ) ;
#5853 = AXIS2_PLACEMENT_3D ( 'NONE', #19062, #10687, #7389 ) ;
#5854 = ADVANCED_FACE ( 'NONE', ( #18923 ), #15293, .T. ) ;
#5855 = CARTESIAN_POINT ( 'NONE',  ( 17.48807464456866256, 131.8965856249792523, 2.656420782620954935 ) ) ;
#5856 = VECTOR ( 'NONE', #16236, 1000.000000000000227 ) ;
#5857 = ORIENTED_EDGE ( 'NONE', *, *, #3006, .T. ) ;
#5858 = CARTESIAN_POINT ( 'NONE',  ( 38.01140435219951996, 113.6344580088725849, 32.58608133808903773 ) ) ;
#5859 = DIRECTION ( 'NONE',  ( 1.000000000000000000, -0.000000000000000000, -0.000000000000000000 ) ) ;
#5860 = EDGE_CURVE ( 'NONE', #4860, #13585, #71, .T. ) ;
#5861 = CARTESIAN_POINT ( 'NONE',  ( 38.58424406990784661, 78.52977050742730114, 35.64915139335016647 ) ) ;
#5862 = CARTESIAN_POINT ( 'NONE',  ( 41.64333658814960870, 134.5151871740939953, 30.00020018409699318 ) ) ;
#5863 = CARTESIAN_POINT ( 'NONE',  ( 38.96631938032478359, 91.01049967264873430, 37.14960608071593384 ) ) ;
#5864 = CARTESIAN_POINT ( 'NONE',  ( 14.15704070161504369, 138.3271338521546454, 9.720138693322796897 ) ) ;
#5865 = CARTESIAN_POINT ( 'NONE',  ( 38.01123955261142129, 95.41221383034442738, 34.53828804502999361 ) ) ;
#5866 = CARTESIAN_POINT ( 'NONE',  ( -151.4692556286852891, -162.2391397928654442, 39.14238933923362396 ) ) ;
#5867 = AXIS2_PLACEMENT_3D ( 'NONE', #666, #14104, #10384 ) ;
#5868 = CARTESIAN_POINT ( 'NONE',  ( 47.05648932407426344, 158.5104996726487343, 31.27175355779120025 ) ) ;
#5869 = CARTESIAN_POINT ( 'NONE',  ( 43.80332655382222384, 96.61133943119284595, 39.21067981925354928 ) ) ;
#5870 = CARTESIAN_POINT ( 'NONE',  ( -157.6495955161842062, -163.1130981290893374, 58.16351966513671812 ) ) ;
#5871 = VERTEX_POINT ( 'NONE', #8794 ) ;
#5872 = CARTESIAN_POINT ( 'NONE',  ( 43.01140435219951286, 74.62977050742732388, 29.55568802177586463 ) ) ;
#5873 = CARTESIAN_POINT ( 'NONE',  ( 71.53613896966024299, 138.8348963267899592, -2.065403804986401859 ) ) ;
#5874 = CARTESIAN_POINT ( 'NONE',  ( -154.3824083646099439, -190.5584106276440650, 58.62277379824867296 ) ) ;
#5875 = EDGE_LOOP ( 'NONE', ( #15537, #17424, #3154, #11551 ) ) ;
#5876 = CARTESIAN_POINT ( 'NONE',  ( 38.01140435219952707, 68.93445800887255359, 35.83527830041809636 ) ) ;
#5877 = CARTESIAN_POINT ( 'NONE',  ( 47.05648932407426344, 123.9844580088725934, 37.14960608071593384 ) ) ;
#5878 = CARTESIAN_POINT ( 'NONE',  ( 41.64333658814960870, 131.7797705074273154, 30.00020018409699318 ) ) ;
#5879 = EDGE_LOOP ( 'NONE', ( #11487, #4308, #2519, #14282 ) ) ;
#5880 = FACE_OUTER_BOUND ( 'NONE', #14790, .T. ) ;
#5881 = VERTEX_POINT ( 'NONE', #13950 ) ;
#5882 = VECTOR ( 'NONE', #3709, 1000.000000000000000 ) ;
#5883 = CARTESIAN_POINT ( 'NONE',  ( 45.74753988029933538, 125.3297705074273125, 30.44471234641811819 ) ) ;
#5884 = CARTESIAN_POINT ( 'NONE',  ( 43.01140435219951996, 170.7104996726487514, 39.21067981925356349 ) ) ;
#5885 = CARTESIAN_POINT ( 'NONE',  ( 40.27526882409969033, 87.82977050742732672, 37.97664729208901946 ) ) ;
#5886 = CARTESIAN_POINT ( 'NONE',  ( 43.01140435219951996, 10.71049967264875491, 34.21067981925357060 ) ) ;
#5887 = CARTESIAN_POINT ( 'NONE',  ( -120.0322075325610598, -126.9891397928655010, -54.65701158161630246 ) ) ;
#5888 = CARTESIAN_POINT ( 'NONE',  ( -141.4692556286852891, -187.1391397928654499, 52.90620854394536821 ) ) ;
#5889 = AXIS2_PLACEMENT_3D ( 'NONE', #15788, #19320, #17334 ) ;
#5890 = CARTESIAN_POINT ( 'NONE',  ( 44.55648932407425633, 133.8844580088725706, 29.45539723777780239 ) ) ;
#5891 = CARTESIAN_POINT ( 'NONE',  ( 11.17254549292281318, -61.68114226949890622, 30.00000000000000000 ) ) ;
#5892 = CARTESIAN_POINT ( 'NONE',  ( -159.5594255724347761, -157.8630981290893089, 43.77915905869157598 ) ) ;
#5893 = APPLICATION_PROTOCOL_DEFINITION ( 'draft international standard', 'automotive_design', 1998, #12800 ) ;
#5894 = CARTESIAN_POINT ( 'NONE',  ( 46.10157429594899270, 108.8344580088725735, 38.46393386101375711 ) ) ;
#5895 = CARTESIAN_POINT ( 'NONE',  ( 44.55648932407425633, 136.8844580088725706, 29.45539723777780239 ) ) ;
#5896 = CARTESIAN_POINT ( 'NONE',  ( 47.43856463449117200, 115.7297705074273324, 35.64915139335016647 ) ) ;
#5897 = CARTESIAN_POINT ( 'NONE',  ( 62.98455118117477980, 139.9299249275418617, 10.79496628861178387 ) ) ;
#5898 = CARTESIAN_POINT ( 'NONE',  ( -148.5561028927606344, -188.7938272943107449, 40.69124936498395328 ) ) ;
#5899 = CARTESIAN_POINT ( 'NONE',  ( 44.37947211624943833, 97.01518717409400949, 38.42115945441014446 ) ) ;
#5900 = CIRCLE ( 'NONE', #2384, 10.00000000000000888 ) ;
#5901 = DIRECTION ( 'NONE',  ( -0.000000000000000000, -0.000000000000000000, 1.000000000000000000 ) ) ;
#5902 = ORIENTED_EDGE ( 'NONE', *, *, #18492, .T. ) ;
#5903 = CARTESIAN_POINT ( 'NONE',  ( 41.46631938032478359, 88.31049967264874567, 38.96596240072933170 ) ) ;
#5904 = CARTESIAN_POINT ( 'NONE',  ( 43.80529445460960858, 154.1304981347762748, -3.137004163733609907 ) ) ;
#5905 = CARTESIAN_POINT ( 'NONE',  ( 24.58042389364637259, 98.66975071380154816, -11.79164420265881574 ) ) ;
#5906 = EDGE_CURVE ( 'NONE', #3622, #9753, #14277, .T. ) ;
#5907 = CARTESIAN_POINT ( 'NONE',  ( -151.4692556286852607, -168.2391397928654442, 39.65701158161629536 ) ) ;
#5908 =( REPRESENTATION_RELATIONSHIP ('NONE','NONE', #6933, #1720 ) REPRESENTATION_RELATIONSHIP_WITH_TRANSFORMATION ( #5125 )SHAPE_REPRESENTATION_RELATIONSHIP( ) );
#5909 = CARTESIAN_POINT ( 'NONE',  ( 43.01140435219951286, 74.62977050742732388, 29.55568802177586107 ) ) ;
#5910 = ORIENTED_EDGE ( 'NONE', *, *, #20563, .T. ) ;
#5911 = ORIENTED_EDGE ( 'NONE', *, *, #8916, .T. ) ;
#5912 = CARTESIAN_POINT ( 'NONE',  ( 39.42975644700377558, 159.0797705074273267, 31.60846029578754468 ) ) ;
#5913 = DIRECTION ( 'NONE',  ( -0.000000000000000000, 1.000000000000000000, -0.000000000000000000 ) ) ;
#5914 = CARTESIAN_POINT ( 'NONE',  ( 46.10157429594899270, 118.7604996726487201, 38.46393386101376421 ) ) ;
#5916 = CARTESIAN_POINT ( 'NONE',  ( 11.06625761453251933, 131.9899775861109106, 3.486483074593720755 ) ) ;
#5915 = CARTESIAN_POINT ( 'NONE',  ( 38.58424406990786082, 75.11518717409400381, 34.21067981925357060 ) ) ;
#5917 = EDGE_CURVE ( 'NONE', #19660, #2439, #3153, .T. ) ;
#5918 = CARTESIAN_POINT ( 'NONE',  ( -142.0420953463935803, -171.5438272943106881, 52.72008163687743831 ) ) ;
#5919 = CARTESIAN_POINT ( 'NONE',  ( 9.976645104453018220, 110.9295780357170571, 15.79146183154218619 ) ) ;
#5920 = CARTESIAN_POINT ( 'NONE',  ( -148.3790856849358306, -189.6630981290893203, 59.16757674456786020 ) ) ;
#5921 = DIRECTION ( 'NONE',  ( -0.3428981916074304581, 0.9393725726208712601, 0.000000000000000000 ) ) ;
#5922 = CARTESIAN_POINT ( 'NONE',  ( 38.01140435219952707, 149.6344580088725991, 32.58608133808903773 ) ) ;
#5923 = CARTESIAN_POINT ( 'NONE',  ( 41.64333658814960870, 138.9797705074273324, 38.42115945441014446 ) ) ;
#5924 = CARTESIAN_POINT ( 'NONE',  ( 76.06694498870253085, 129.1134374410657983, 4.287174360044270216 ) ) ;
#5925 = CARTESIAN_POINT ( 'NONE',  ( 39.42975644700377558, 122.8151871740940067, 31.60846029578754468 ) ) ;
#5926 = SURFACE_STYLE_USAGE ( .BOTH. , #2616 ) ;
#5927 = CARTESIAN_POINT ( 'NONE',  ( -157.2955611005345986, -158.6084106276439911, 41.63779006702063867 ) ) ;
#5928 = CARTESIAN_POINT ( 'NONE',  ( -161.4692556286852891, -164.6391397928654499, 46.40781461928724383 ) ) ;
#5929 = CARTESIAN_POINT ( 'NONE',  ( -151.4692556286852607, -156.2391397928654726, 39.65701158161629536 ) ) ;
#5930 = CARTESIAN_POINT ( 'NONE',  ( 37.19530960600651071, 92.23011878076297876, 13.65210914576621271 ) ) ;
#5931 = FACE_OUTER_BOUND ( 'NONE', #7696, .T. ) ;
#5932 = CARTESIAN_POINT ( 'NONE',  ( 41.64333658814960870, 107.5151871740939953, 30.00020018409699318 ) ) ;
#5933 = EDGE_LOOP ( 'NONE', ( #9070, #17560, #8614, #10670 ) ) ;
#5934 = CYLINDRICAL_SURFACE ( 'NONE', #15221, 4.999999999999997335 ) ;
#5935 = EDGE_CURVE ( 'NONE', #16834, #13122, #5400, .T. ) ;
#5936 = ORIENTED_EDGE ( 'NONE', *, *, #19264, .F. ) ;
#5937 = CARTESIAN_POINT ( 'NONE',  ( 43.01140435219951286, 90.53445800887259054, 39.46799094044489209 ) ) ;
#5938 = DIRECTION ( 'NONE',  ( -0.000000000000000000, 1.000000000000000000, -0.000000000000000000 ) ) ;
#5939 = CARTESIAN_POINT ( 'NONE',  ( 43.01140435219951286, 152.9604996726487514, 28.95336869806222779 ) ) ;
#5941 = CARTESIAN_POINT ( 'NONE',  ( 31.68064667488295783, 94.17100518331969283, -5.125072385659846574 ) ) ;
#5940 = CARTESIAN_POINT ( 'NONE',  ( 45.74753988029933538, 110.0651871740939782, 30.44471234641811819 ) ) ;
#5942 = CARTESIAN_POINT ( 'NONE',  ( 46.10157429594899270, 65.66049967264873999, 29.95742577749337343 ) ) ;
#5944 = CARTESIAN_POINT ( 'NONE',  ( -149.8854112254399240, -182.3899795514095672, 39.65701158161629536 ) ) ;
#5943 = DIRECTION ( 'NONE',  ( -1.000000000000000000, 0.000000000000000000, 0.000000000000000000 ) ) ;
#5945 = AXIS2_PLACEMENT_3D ( 'NONE', #2628, #13908, #15568 ) ;
#5946 = DIRECTION ( 'NONE',  ( -1.000000000000000000, 0.000000000000000000, 0.000000000000000000 ) ) ;
#5947 = CARTESIAN_POINT ( 'NONE',  ( 43.01140435219951286, 116.0344580088725763, 29.21067981925356705 ) ) ;
#5948 = CARTESIAN_POINT ( 'NONE',  ( 41.64333658814960870, 71.51518717409399528, 30.00020018409699318 ) ) ;
#5949 = CARTESIAN_POINT ( 'NONE',  ( 38.58424406990785371, 152.9651871740940123, 32.77220824515697473 ) ) ;
#5950 = DIRECTION ( 'NONE',  ( -1.000000000000000000, 0.000000000000000000, 0.000000000000000000 ) ) ;
#5951 = CARTESIAN_POINT ( 'NONE',  ( -143.8425227516148084, -168.0938272943107563, 44.11586579668791330 ) ) ;
#5952 = CARTESIAN_POINT ( 'NONE',  ( -142.0420953463936087, -195.6584106276440593, 49.65701158161630957 ) ) ;
#5953 = ADVANCED_FACE ( 'NONE', ( #7031 ), #2065, .F. ) ;
#5954 = ORIENTED_EDGE ( 'NONE', *, *, #4813, .F. ) ;
#5955 = CARTESIAN_POINT ( 'NONE',  ( -157.2955611005346270, -178.7084106276440139, 57.67623309621198047 ) ) ;
#5956 = CARTESIAN_POINT ( 'NONE',  ( 20.33033954036769941, 94.15838586645493535, 7.144317217164116052 ) ) ;
#5957 = ORIENTED_EDGE ( 'NONE', *, *, #7246, .F. ) ;
#5958 = CARTESIAN_POINT ( 'NONE',  ( 46.59305225739526435, 133.9151871740940010, 31.60846029578754468 ) ) ;
#5959 = CARTESIAN_POINT ( 'NONE',  ( 47.43856463449118621, 154.6151871740940180, 34.21067981925357060 ) ) ;
#5960 = EDGE_CURVE ( 'NONE', #10863, #7143, #3394, .T. ) ;
#5961 = CARTESIAN_POINT ( 'NONE',  ( 44.37947211624943833, 100.2797705074273154, 38.42115945441014446 ) ) ;
#5962 = ORIENTED_EDGE ( 'NONE', *, *, #12310, .F. ) ;
#5963 = ORIENTED_EDGE ( 'NONE', *, *, #10314, .T. ) ;
#5964 = CARTESIAN_POINT ( 'NONE',  ( 19.52755003174225124, 104.2962547294809070, 15.51356631106660089 ) ) ;
#5965 = VERTEX_POINT ( 'NONE', #20902 ) ;
#5966 = CARTESIAN_POINT ( 'NONE',  ( 46.10157429594899270, 111.8344580088725735, 38.46393386101376421 ) ) ;
#5967 = DIRECTION ( 'NONE',  ( 0.000000000000000000, -1.000000000000000000, 0.000000000000000000 ) ) ;
#5968 = CARTESIAN_POINT ( 'NONE',  ( 43.01140435219951286, 73.12977050742729546, 38.86567161673127657 ) ) ;
#5969 = CARTESIAN_POINT ( 'NONE',  ( 43.01140435219951286, 131.3651871740940180, 29.55568802177586463 ) ) ;
#5970 = CARTESIAN_POINT ( 'NONE',  ( 48.01140435219951996, 95.06049967264874567, 35.83527830041810347 ) ) ;
#5971 = CARTESIAN_POINT ( 'NONE',  ( 34.41316853928974950, 153.0433231119815503, 10.55326060710041958 ) ) ;
#5972 = CARTESIAN_POINT ( 'NONE',  ( 40.78964507673602924, 95.00417210663486856, 38.70176206714167932 ) ) ;
#5973 = CARTESIAN_POINT ( 'NONE',  ( -159.5594255724347761, -158.7891397928654555, 43.77915905869157598 ) ) ;
#5974 =( BOUNDED_CURVE ( )  B_SPLINE_CURVE ( 2, ( #21124, #2385, #7462, #7359, #20904, #20796, #6008, #9122, #11188, #7689, #12844, #19562, #12737 ),
 .UNSPECIFIED., .F., .F. ) 
 B_SPLINE_CURVE_WITH_KNOTS ( ( 3, 2, 2, 2, 2, 2, 3 ),
 ( 0.7678571428571427937, 0.7714285714285714635, 0.7785714285714285809, 0.7857142857142856984, 0.7928571428571428159, 0.8000000000000000444, 0.8035714285714286031 ),
 .UNSPECIFIED. ) 
 CURVE ( )  GEOMETRIC_REPRESENTATION_ITEM ( )  RATIONAL_B_SPLINE_CURVE ( ( 0.9755282581475768211, 0.9755282581475763770, 1.000000000000000000, 0.9510565162951535312, 1.000000000000000000, 0.9510565162951535312, 1.000000000000000000, 0.9510565162951535312, 1.000000000000000000, 0.9510565162951535312, 1.000000000000000000, 0.9755282581475768211, 0.9755282581475768211 ) ) 
 REPRESENTATION_ITEM ( '' )  );
#5975 = CARTESIAN_POINT ( 'NONE',  ( 39.92123440845005433, 152.3344580088725593, 29.95742577749336988 ) ) ;
#5976 = FACE_OUTER_BOUND ( 'NONE', #4020, .T. ) ;
#5977 = CARTESIAN_POINT ( 'NONE',  ( 48.01140435219951996, 106.4344580088725678, 32.58608133808903773 ) ) ;
#5978 = AXIS2_PLACEMENT_3D ( 'NONE', #297, #20469, #5362 ) ;
#5979 = ORIENTED_EDGE ( 'NONE', *, *, #16206, .F. ) ;
#5980 = CARTESIAN_POINT ( 'NONE',  ( 46.59305225739526435, 76.57977050742731251, 36.81289934271958941 ) ) ;
#5981 = CARTESIAN_POINT ( 'NONE',  ( -143.8425227516148084, -165.0938272943107279, 44.11586579668791330 ) ) ;
#5982 = CARTESIAN_POINT ( 'NONE',  ( 73.40451243997107156, 135.6611253642151098, -1.946480675884423084 ) ) ;
#5983 = CARTESIAN_POINT ( 'NONE',  ( -159.0959885057557983, -194.4584106276440423, 44.11586579668791330 ) ) ;
#5984 = VERTEX_POINT ( 'NONE', #6006 ) ;
#5985 = PLANE ( 'NONE',  #4431 ) ;
#5986 = FACE_OUTER_BOUND ( 'NONE', #1665, .T. ) ;
#5987 = CARTESIAN_POINT ( 'NONE',  ( 39.42975644700377558, 120.6797705074273210, 36.81289934271958941 ) ) ;
#5988 = ORIENTED_EDGE ( 'NONE', *, *, #6212, .T. ) ;
#5989 = FACE_OUTER_BOUND ( 'NONE', #10586, .T. ) ;
#5990 = ORIENTED_EDGE ( 'NONE', *, *, #1181, .T. ) ;
#5991 = CARTESIAN_POINT ( 'NONE',  ( 44.37947211624943833, 122.4797705074273182, 30.00020018409699318 ) ) ;
#5992 = CARTESIAN_POINT ( 'NONE',  ( 46.10157429594899270, 109.7604996726487343, 38.46393386101375711 ) ) ;
#5993 = DIRECTION ( 'NONE',  ( 0.000000000000000000, 1.000000000000000000, 0.000000000000000000 ) ) ;
#5994 = DIRECTION ( 'NONE',  ( -0.9385982292947087080, -0.3450121214752279730, -0.000000000000000000 ) ) ;
#5995 = CARTESIAN_POINT ( 'NONE',  ( 11.17254549292281673, -61.68114226949890622, -16.21320343559643717 ) ) ;
#5996 = CARTESIAN_POINT ( 'NONE',  ( -143.3790856849358306, -193.2891397928654555, 55.53486410454105027 ) ) ;
#5997 = CARTESIAN_POINT ( 'NONE',  ( 43.01140435219951286, 67.46049967264873715, 39.21067981925356349 ) ) ;
#5998 = CARTESIAN_POINT ( 'NONE',  ( 47.05648932407426344, 124.9104996726487542, 37.14960608071593384 ) ) ;
#5999 = CARTESIAN_POINT ( 'NONE',  ( -157.6495955161842062, -158.0130981290893146, 41.15050349809590102 ) ) ;
#6000 = PRODUCT_CONTEXT ( 'NONE', #15354, 'mechanical' ) ;
#6001 = EDGE_CURVE ( 'NONE', #20293, #11358, #4348, .T. ) ;
#6002 = ADVANCED_FACE ( 'NONE', ( #19033 ), #16145, .T. ) ;
#6003 = CARTESIAN_POINT ( 'NONE',  ( 41.46631938032478359, 132.3844580088725706, 38.96596240072933170 ) ) ;
#6004 = CARTESIAN_POINT ( 'NONE',  ( 44.37947211624943833, 107.4797705074273182, 30.00020018409699318 ) ) ;
#6005 = CARTESIAN_POINT ( 'NONE',  ( 70.99289463508769416, 124.0080672713295087, 11.50917073501047483 ) ) ;
#6006 = CARTESIAN_POINT ( 'NONE',  ( 43.01140435219951286, 89.96049967264873715, 29.21067981925356705 ) ) ;
#6007 = CARTESIAN_POINT ( 'NONE',  ( 38.58424406990785371, 101.9651871740939981, 32.77220824515697473 ) ) ;
#6008 = CARTESIAN_POINT ( 'NONE',  ( -141.4692556286852891, -162.0630981290892976, 49.65701158161630957 ) ) ;
#6009 = EDGE_LOOP ( 'NONE', ( #14956, #2495, #7852, #4411 ) ) ;
#6010 = CARTESIAN_POINT ( 'NONE',  ( 41.46631938032478359, 87.11049967264874283, 29.45539723777780239 ) ) ;
#6011 = CARTESIAN_POINT ( 'NONE',  ( 42.92180000979148957, 85.67454126555050209, 7.339147150375312734 ) ) ;
#6012 = CARTESIAN_POINT ( 'NONE',  ( 26.96882349746146446, 96.81297435472995971, -11.91061488385382106 ) ) ;
#6013 = CARTESIAN_POINT ( 'NONE',  ( 28.88048086162541850, 151.0887240815949895, -10.63664014359656385 ) ) ;
#6014 = CARTESIAN_POINT ( 'NONE',  ( 45.74753988029934249, 73.42977050742730682, 37.97664729208901235 ) ) ;
#6015 = VERTEX_POINT ( 'NONE', #4145 ) ;
#6016 = ORIENTED_EDGE ( 'NONE', *, *, #10822, .T. ) ;
#6017 = CARTESIAN_POINT ( 'NONE',  ( 44.37947211624943833, 152.4797705074273324, 30.00020018409699318 ) ) ;
#6018 = CARTESIAN_POINT ( 'NONE',  ( 107.0370895198517189, 343.6663954850758955, -3.999999999999996447 ) ) ;
#6019 = VERTEX_POINT ( 'NONE', #21122 ) ;
#6020 = CARTESIAN_POINT ( 'NONE',  ( 38.01140435219952707, 120.7104996726487371, 34.21067981925357060 ) ) ;
#6022 = CARTESIAN_POINT ( 'NONE',  ( 58.73109577922829061, 150.2274887891485662, -1.632724326791204605 ) ) ;
#6021 = CARTESIAN_POINT ( 'NONE',  ( 43.01140435219951286, 75.86518717409398960, 38.86567161673127657 ) ) ;
#6023 = CARTESIAN_POINT ( 'NONE',  ( -160.8964159109769696, -176.0438272943106881, 46.59394152635518083 ) ) ;
#6024 = CARTESIAN_POINT ( 'NONE',  ( 41.61242760320212852, 154.1118385459532760, 10.79173905232880237 ) ) ;
#6025 = CARTESIAN_POINT ( 'NONE',  ( -161.4692556286852607, -187.7130981290893033, 46.40781461928724383 ) ) ;
#6026 = ADVANCED_FACE ( 'NONE', ( #17579 ), #767, .T. ) ;
#6027 = CARTESIAN_POINT ( 'NONE',  ( -94.10404323627655288, -13.18023274290474767, 4.000000000000021316 ) ) ;
#6028 = CARTESIAN_POINT ( 'NONE',  ( 147.8787791192428074, -136.9891397928655010, 0.3429884183836981459 ) ) ;
#6029 = CARTESIAN_POINT ( 'NONE',  ( 46.59305225739526435, 136.5797705074272983, 36.81289934271958941 ) ) ;
#6030 = CARTESIAN_POINT ( 'NONE',  ( 13.73412108254838238, 102.0109333093626134, 0.4776103675054816922 ) ) ;
#6031 = CARTESIAN_POINT ( 'NONE',  ( 38.58424406990785371, 123.2651871740939953, 35.64915139335015937 ) ) ;
#6032 = CARTESIAN_POINT ( 'NONE',  ( 48.01140435219951996, 137.2104996726487514, 34.21067981925357060 ) ) ;
#6033 = CARTESIAN_POINT ( 'NONE',  ( 38.96631938032478359, 151.0104996726487343, 37.14960608071593384 ) ) ;
#6034 = APPLICATION_CONTEXT ( 'automotive_design' ) ;
#6035 = AXIS2_PLACEMENT_3D ( 'NONE', #12713, #6092, #9638 ) ;
#6036 = CARTESIAN_POINT ( 'NONE',  ( 48.01140435219951996, 149.0604996726487173, 35.83527830041809636 ) ) ;
#6037 = CARTESIAN_POINT ( 'NONE',  ( 42.59292608294269655, 91.62918162712271908, 20.43785202907404752 ) ) ;
#6038 = CARTESIAN_POINT ( 'NONE',  ( 46.10157429594899270, 82.76049967264874851, 38.46393386101375711 ) ) ;
#6039 = VECTOR ( 'NONE', #15498, 1000.000000000000227 ) ;
#6040 = CARTESIAN_POINT ( 'NONE',  ( 43.01140435219951286, 108.8651871740939896, 38.86567161673127657 ) ) ;
#6041 = ORIENTED_EDGE ( 'NONE', *, *, #11554, .F. ) ;
#6042 = CARTESIAN_POINT ( 'NONE',  ( -151.4692556286852607, -157.7391397928654726, 59.65701158161632378 ) ) ;
#6043 = EDGE_LOOP ( 'NONE', ( #20752, #18902, #4735, #19873 ) ) ;
#6044 = CARTESIAN_POINT ( 'NONE',  ( 47.05648932407426344, 93.98445800887257917, 37.14960608071593384 ) ) ;
#6045 = DIRECTION ( 'NONE',  ( 0.000000000000000000, 0.000000000000000000, 1.000000000000000000 ) ) ;
#6046 = PRODUCT_DEFINITION_SHAPE ( 'NONE', 'NONE',  #14706 ) ;
#6047 = AXIS2_PLACEMENT_3D ( 'NONE', #8300, #21748, #1793 ) ;
#6048 = AXIS2_PLACEMENT_3D ( 'NONE', #18233, #13494, #3135 ) ;
#6049 = CARTESIAN_POINT ( 'NONE',  ( 39.92123440845004723, 151.1604996726487116, 38.46393386101376421 ) ) ;
#6051 = CARTESIAN_POINT ( 'NONE',  ( 15.53781593631592983, 113.9137188375014347, -11.07707013084618097 ) ) ;
#6050 = CARTESIAN_POINT ( 'NONE',  ( 41.64333658814960870, 104.5151871740939953, 30.00020018409699318 ) ) ;
#6052 = CARTESIAN_POINT ( 'NONE',  ( 48.01140435219951996, 62.36049967264873573, 32.58608133808903773 ) ) ;
#6054 = DIRECTION ( 'NONE',  ( 0.000000000000000000, 1.000000000000000000, 0.000000000000000000 ) ) ;
#6053 = DIRECTION ( 'NONE',  ( 0.000000000000000000, 0.000000000000000000, -1.000000000000000000 ) ) ;
#6055 = LINE ( 'NONE', #2426, #3821 ) ;
#6056 = DIRECTION ( 'NONE',  ( 0.000000000000000000, 0.000000000000000000, 1.000000000000000000 ) ) ;
#6057 = CARTESIAN_POINT ( 'NONE',  ( 43.01140435219951286, 59.03445800887258343, 29.21067981925356705 ) ) ;
#6058 = CARTESIAN_POINT ( 'NONE',  ( 39.42975644700377558, 69.41518717409400097, 36.81289934271958941 ) ) ;
#6059 = CARTESIAN_POINT ( 'NONE',  ( 54.54805624998882507, 152.1374805055981199, -2.779977617235711129 ) ) ;
#6060 = CARTESIAN_POINT ( 'NONE',  ( 41.64333658814960870, 153.7151871740940123, 38.42115945441014446 ) ) ;
#6061 = CARTESIAN_POINT ( 'NONE',  ( 157.5268905834513475, 193.0332408774651185, 272.0939500981630204 ) ) ;
#6062 = CARTESIAN_POINT ( 'NONE',  ( -143.8425227516148084, -171.0938272943107279, 44.11586579668791330 ) ) ;
#6063 = CARTESIAN_POINT ( 'NONE',  ( -160.8964159109769696, -185.0084106276440536, 52.72008163687743121 ) ) ;
#6064 = EDGE_LOOP ( 'NONE', ( #11495, #7796, #20088, #5857 ) ) ;
#6065 = CARTESIAN_POINT ( 'NONE',  ( -142.0420953463935803, -168.8084106276440650, 52.72008163687743831 ) ) ;
#6066 = CARTESIAN_POINT ( 'NONE',  ( 8.804574439154260190, 117.1883747968346654, 15.00137004459121393 ) ) ;
#6067 = CYLINDRICAL_SURFACE ( 'NONE', #17256, 10.00000000000000888 ) ;
#6068 = CARTESIAN_POINT ( 'NONE',  ( 41.64333658814960870, 135.7151871740940123, 38.42115945441014446 ) ) ;
#6069 = CARTESIAN_POINT ( 'NONE',  ( 40.27526882409969744, 156.5651871740939782, 37.97664729208901235 ) ) ;
#6070 = CARTESIAN_POINT ( 'NONE',  ( 46.59305225739526435, 92.17977050742732104, 31.60846029578754468 ) ) ;
#6071 = ORIENTED_EDGE ( 'NONE', *, *, #13052, .F. ) ;
#6072 = EDGE_LOOP ( 'NONE', ( #21296, #6121, #13350, #6205 ) ) ;
#6073 = CARTESIAN_POINT ( 'NONE',  ( 48.35156950851215640, 92.21792820573091376, 14.20396468032920012 ) ) ;
#6074 = EDGE_CURVE ( 'NONE', #10182, #4977, #436, .T. ) ;
#6075 = ORIENTED_EDGE ( 'NONE', *, *, #17476, .T. ) ;
#6076 = CARTESIAN_POINT ( 'NONE',  ( 46.10157429594899270, 117.8344580088725451, 38.46393386101376421 ) ) ;
#6077 = CARTESIAN_POINT ( 'NONE',  ( -91.10645082872859746, 10.96617311717548660, 4.000000000000021316 ) ) ;
#6078 = CARTESIAN_POINT ( 'NONE',  ( 39.42975644700377558, 72.67977050742730682, 36.81289934271958941 ) ) ;
#6079 = CARTESIAN_POINT ( 'NONE',  ( 44.37947211624943833, 133.0151871740939953, 38.42115945441014446 ) ) ;
#6080 = CARTESIAN_POINT ( 'NONE',  ( 38.96631938032478359, 88.01049967264874851, 37.14960608071593384 ) ) ;
#6081 = CARTESIAN_POINT ( 'NONE',  ( 38.04450641318627646, 95.40535984405393322, 33.55020052675506292 ) ) ;
#6082 = CARTESIAN_POINT ( 'NONE',  ( -145.2889157411863721, -160.4391397928654328, 58.16351966513671812 ) ) ;
#6083 = CARTESIAN_POINT ( 'NONE',  ( 129.2454342010813662, 193.1635054290503319, -29.99999999999997868 ) ) ;
#6084 = CARTESIAN_POINT ( 'NONE',  ( 48.01140435219951996, 142.1344580088725991, 35.83527830041809636 ) ) ;
#6085 = ORIENTED_EDGE ( 'NONE', *, *, #10169, .F. ) ;
#6086 = CARTESIAN_POINT ( 'NONE',  ( 45.74753988029933538, 71.32977050742732672, 30.44471234641811819 ) ) ;
#6087 = CARTESIAN_POINT ( 'NONE',  ( -159.0959885057557983, -158.1938272943107222, 44.11586579668791330 ) ) ;
#6088 = CARTESIAN_POINT ( 'NONE',  ( 23.67598417054553295, 91.65793073385727041, -5.994147020910363999 ) ) ;
#6089 = CARTESIAN_POINT ( 'NONE',  ( -145.6429501568359797, -195.2084106276440707, 41.63779006702063867 ) ) ;
#6090 = ORIENTED_EDGE ( 'NONE', *, *, #4408, .F. ) ;
#6091 = CARTESIAN_POINT ( 'NONE',  ( -153.0531000319306827, -160.8160212151857138, 59.65701158161631668 ) ) ;
#6092 = DIRECTION ( 'NONE',  ( -0.000000000000000000, 1.000000000000000000, -0.000000000000000000 ) ) ;
#6093 = CARTESIAN_POINT ( 'NONE',  ( 47.43856463449117911, 124.7297705074273182, 35.64915139335015937 ) ) ;
#6094 = VERTEX_POINT ( 'NONE', #4473 ) ;
#6095 = ORIENTED_EDGE ( 'NONE', *, *, #26, .T. ) ;
#6096 = CARTESIAN_POINT ( 'NONE',  ( 44.37947211624943833, 127.2797705074273438, 38.42115945441014446 ) ) ;
#6097 = CARTESIAN_POINT ( 'NONE',  ( 45.05628966327351748, 58.83593637268779730, 29.61779221216752944 ) ) ;
#6098 = CARTESIAN_POINT ( 'NONE',  ( 46.10157429594899270, 63.83445800887258770, 38.46393386101376421 ) ) ;
#6099 =( BOUNDED_CURVE ( )  B_SPLINE_CURVE ( 2, ( #14387, #14064, #12524, #21127, #7464, #17477, #14173, #12298, #15608, #7253, #2387, #15821, #18928 ),
 .UNSPECIFIED., .F., .T. ) 
 B_SPLINE_CURVE_WITH_KNOTS ( ( 3, 2, 2, 2, 2, 2, 3 ),
 ( 0.007352941176470595940, 0.008823529411764705760, 0.01176470588235294101, 0.01470588235294117627, 0.01764705882352941152, 0.02058823529411764677, 0.02205882352941176960 ),
 .UNSPECIFIED. ) 
 CURVE ( )  GEOMETRIC_REPRESENTATION_ITEM ( )  RATIONAL_B_SPLINE_CURVE ( ( 0.9755282581475767101, 0.9755282581475768211, 1.000000000000000000, 0.9510565162951535312, 1.000000000000000000, 0.9510565162951535312, 1.000000000000000000, 0.9510565162951535312, 1.000000000000000000, 0.9510565162951535312, 1.000000000000000000, 0.9755282581475765991, 0.9755282581475767101 ) ) 
 REPRESENTATION_ITEM ( '' )  );
#6100 = EDGE_CURVE ( 'NONE', #13353, #2795, #7674, .T. ) ;
#6101 = LINE ( 'NONE', #12831, #11154 ) ;
#6102 = CARTESIAN_POINT ( 'NONE',  ( 39.92123440845005433, 102.2344580088725650, 38.46393386101375711 ) ) ;
#6103 = DIRECTION ( 'NONE',  ( 1.000000000000000000, -0.000000000000000000, -0.000000000000000000 ) ) ;
#6104 = CARTESIAN_POINT ( 'NONE',  ( -148.3790856849358306, -190.5891397928654953, 59.16757674456786020 ) ) ;
#6105 = EDGE_CURVE ( 'NONE', #20206, #561, #8184, .T. ) ;
#6106 = DIRECTION ( 'NONE',  ( 1.000000000000000000, 0.000000000000000000, 0.000000000000000000 ) ) ;
#6107 = CARTESIAN_POINT ( 'NONE',  ( 46.10157429594899270, 94.73445800887257917, 29.95742577749336988 ) ) ;
#6108 = CARTESIAN_POINT ( 'NONE',  ( -142.0420953463935803, -189.5438272943106881, 52.72008163687743831 ) ) ;
#6109 = CARTESIAN_POINT ( 'NONE',  ( 38.96631938032478359, 125.4844580088725934, 31.27175355779120025 ) ) ;
#6110 = CARTESIAN_POINT ( 'NONE',  ( 41.64333658814960870, 105.9797705074273182, 38.42115945441014446 ) ) ;
#6111 = CARTESIAN_POINT ( 'NONE',  ( 32.01435502045076475, 93.85226834503447435, 6.866149820358673495 ) ) ;
#6112 = CARTESIAN_POINT ( 'NONE',  ( -160.8964159109769696, -193.8938272943107393, 49.65701158161630957 ) ) ;
#6113 = CARTESIAN_POINT ( 'NONE',  ( 45.74753988029934249, 98.06518717409399244, 30.44471234641812174 ) ) ;
#6114 = CARTESIAN_POINT ( 'NONE',  ( -97.23064952102208736, 13.78046159333444720, 4.000000000000021316 ) ) ;
#6115 = ORIENTED_EDGE ( 'NONE', *, *, #4612, .T. ) ;
#6116 = CARTESIAN_POINT ( 'NONE',  ( 44.55648932407425633, 128.8104996726487457, 29.45539723777780239 ) ) ;
#6117 = CARTESIAN_POINT ( 'NONE',  ( 61.76154402333882132, 148.5480768402654803, 4.482004293238171400 ) ) ;
#6118 = CARTESIAN_POINT ( 'NONE',  ( 55.45346087869361185, 145.1240540049360845, -8.577242388453932165 ) ) ;
#6119 = CARTESIAN_POINT ( 'NONE',  ( 54.54805624998882507, 152.1374805055981199, -2.779977617235711129 ) ) ;
#6120 = CARTESIAN_POINT ( 'NONE',  ( 45.74753988029934249, 64.42977050742732104, 37.97664729208901235 ) ) ;
#6121 = ORIENTED_EDGE ( 'NONE', *, *, #14025, .T. ) ;
#6122 = ORIENTED_EDGE ( 'NONE', *, *, #17933, .F. ) ;
#6123 = CARTESIAN_POINT ( 'NONE',  ( 38.58424406990784661, 159.2297705074272756, 32.77220824515698183 ) ) ;
#6124 = CARTESIAN_POINT ( 'NONE',  ( -157.6495955161842062, -194.0130981290893146, 41.15050349809589392 ) ) ;
#6125 = VECTOR ( 'NONE', #15117, 1000.000000000000000 ) ;
#6126 = CARTESIAN_POINT ( 'NONE',  ( 48.01140435219951996, 122.3604996726487428, 32.58608133808903773 ) ) ;
#6128 = CARTESIAN_POINT ( 'NONE',  ( 16.16624775068580533, 140.9673012293996237, 10.82561872270659009 ) ) ;
#6127 = CARTESIAN_POINT ( 'NONE',  ( 47.43856463449117200, 67.76518717409399528, 32.77220824515698183 ) ) ;
#6129 = CARTESIAN_POINT ( 'NONE',  ( 43.01140435219951286, 66.53445800887257633, 39.21067981925356349 ) ) ;
#6130 = AXIS2_PLACEMENT_3D ( 'NONE', #14301, #17819, #17606 ) ;
#6131 = CARTESIAN_POINT ( 'NONE',  ( -143.8425227516148084, -174.0938272943107279, 44.11586579668791330 ) ) ;
#6132 = CARTESIAN_POINT ( 'NONE',  ( 49.46632042442519861, 86.28835692931116341, 14.12497754236212977 ) ) ;
#6133 = CARTESIAN_POINT ( 'NONE',  ( -145.2889157411863721, -180.5130981290893146, 58.16351966513671812 ) ) ;
#6134 = DIRECTION ( 'NONE',  ( -1.000000000000000000, -0.000000000000000000, -0.000000000000000000 ) ) ;
#6135 = CARTESIAN_POINT ( 'NONE',  ( 101.4021762516569822, 137.5714195593754710, -35.00000000000000000 ) ) ;
#6136 = CARTESIAN_POINT ( 'NONE',  ( 43.01140435219951286, 137.6297705074273381, 29.55568802177586463 ) ) ;
#6137 = CARTESIAN_POINT ( 'NONE',  ( 26.28242620001017471, 89.94675250444232972, 6.906269859504051922 ) ) ;
#6138 = CARTESIAN_POINT ( 'NONE',  ( 46.59305225739526435, 130.9151871740940010, 31.60846029578754468 ) ) ;
#6139 = DIRECTION ( 'NONE',  ( -0.000000000000000000, 0.000000000000000000, -1.000000000000000000 ) ) ;
#6140 = CARTESIAN_POINT ( 'NONE',  ( 138.4260920561042667, 141.9264758756783351, -5.999999999999976019 ) ) ;
#6141 = DIRECTION ( 'NONE',  ( 0.000000000000000000, 1.000000000000000000, 0.000000000000000000 ) ) ;
#6142 = CARTESIAN_POINT ( 'NONE',  ( 24.78883071187807730, 141.3519591882296709, -10.86778418981948846 ) ) ;
#6143 = CARTESIAN_POINT ( 'NONE',  ( 43.01140435219951286, 75.53445800887257633, 39.21067981925356349 ) ) ;
#6144 = CARTESIAN_POINT ( 'NONE',  ( 43.01140435219951286, 104.3651871740940038, 29.55568802177586463 ) ) ;
#6145 = ORIENTED_EDGE ( 'NONE', *, *, #11081, .T. ) ;
#6146 = CARTESIAN_POINT ( 'NONE',  ( -141.4692556286852891, -156.8391397928654669, 46.40781461928724383 ) ) ;
#6147 = VERTEX_POINT ( 'NONE', #2719 ) ;
#6148 = CARTESIAN_POINT ( 'NONE',  ( 39.92123440845004723, 80.33445800887258770, 29.95742577749337343 ) ) ;
#6149 = DIRECTION ( 'NONE',  ( -0.000000000000000000, -0.000000000000000000, -1.000000000000000000 ) ) ;
#6150 = CARTESIAN_POINT ( 'NONE',  ( 41.46631938032478359, 151.3104996726487457, 38.96596240072933170 ) ) ;
#6152 = CARTESIAN_POINT ( 'NONE',  ( 61.44294336830710535, 141.1433446673695471, 5.708471897238777792 ) ) ;
#6151 = CARTESIAN_POINT ( 'NONE',  ( 40.27526882409969033, 110.6651871740940010, 30.44471234641811819 ) ) ;
#6153 = CARTESIAN_POINT ( 'NONE',  ( 38.01140435219952707, 66.71049967264873715, 34.21067981925357060 ) ) ;
#6155 = CARTESIAN_POINT ( 'NONE',  ( -145.2889157411863437, -183.5130981290892578, 58.16351966513671812 ) ) ;
#6154 = CARTESIAN_POINT ( 'NONE',  ( 47.75558613178728251, 144.4531355194695550, 35.82300994916138848 ) ) ;
#6156 = FILL_AREA_STYLE_COLOUR ( '', #4161 ) ;
#6157 = CARTESIAN_POINT ( 'NONE',  ( -153.0531000319306543, -186.8899795514095672, 59.65701158161632378 ) ) ;
#6158 = CARTESIAN_POINT ( 'NONE',  ( 43.01140435219957681, 71.96049967264872294, 29.21067981925356705 ) ) ;
#6159 =( BOUNDED_CURVE ( )  B_SPLINE_CURVE ( 2, ( #19241, #5785, #9223, #833, #7567, #14267, #21012, #8965, #8753, #575, #15365, #19388, #6882 ),
 .UNSPECIFIED., .F., .F. ) 
 B_SPLINE_CURVE_WITH_KNOTS ( ( 3, 2, 2, 2, 2, 2, 3 ),
 ( 0.2573529411764705621, 0.2588235294117647300, 0.2617647058823529549, 0.2647058823529411797, 0.2676470588235294046, 0.2705882352941176294, 0.2720588235294117974 ),
 .UNSPECIFIED. ) 
 CURVE ( )  GEOMETRIC_REPRESENTATION_ITEM ( )  RATIONAL_B_SPLINE_CURVE ( ( 0.9755282581475768211, 0.9755282581475763770, 1.000000000000000000, 0.9510565162951535312, 1.000000000000000000, 0.9510565162951535312, 1.000000000000000000, 0.9510565162951535312, 1.000000000000000000, 0.9510565162951535312, 1.000000000000000000, 0.9755282581475763770, 0.9755282581475768211 ) ) 
 REPRESENTATION_ITEM ( '' )  );
#6160 = CARTESIAN_POINT ( 'NONE',  ( 45.74753988029933538, 158.3297705074273267, 30.44471234641811819 ) ) ;
#6161 = CARTESIAN_POINT ( 'NONE',  ( 68.88151390383544026, 142.3271613368909811, -9.208263745312144977 ) ) ;
#6162 = CARTESIAN_POINT ( 'NONE',  ( 45.74753988029934249, 152.0651871740939782, 30.44471234641812174 ) ) ;
#6163 = CARTESIAN_POINT ( 'NONE',  ( 48.01140435219951996, 95.06049967264874567, 35.83527830041809636 ) ) ;
#6164 = VECTOR ( 'NONE', #20162, 1000.000000000000000 ) ;
#6165 = CARTESIAN_POINT ( 'NONE',  ( -148.5561028927606344, -167.7938272943107165, 40.69124936498395328 ) ) ;
#6166 = CARTESIAN_POINT ( 'NONE',  ( -142.0420953463936087, -180.6584106276440309, 49.65701158161630957 ) ) ;
#6167 = ORIENTED_EDGE ( 'NONE', *, *, #7870, .F. ) ;
#6168 = CARTESIAN_POINT ( 'NONE',  ( 40.27526882409969744, 69.56518717409400665, 37.97664729208901235 ) ) ;
#6169 = CARTESIAN_POINT ( 'NONE',  ( -154.3824083646099439, -166.5584106276440366, 58.62277379824867296 ) ) ;
#6170 = CARTESIAN_POINT ( 'NONE',  ( 53.27251631713230040, 87.16359876908097704, 20.00146008344694337 ) ) ;
#6171 = CARTESIAN_POINT ( 'NONE',  ( 43.01140435219951996, 10.71049967264875491, 34.21067981925357060 ) ) ;
#6172 = CARTESIAN_POINT ( 'NONE',  ( 40.27526882409969033, 134.6651871740940294, 30.44471234641811819 ) ) ;
#6173 = CARTESIAN_POINT ( 'NONE',  ( 45.74753988029934249, 157.1651871740940010, 37.97664729208901235 ) ) ;
#6174 = CARTESIAN_POINT ( 'NONE',  ( 61.38527826276358468, 91.11739401521901982, -13.29920278214092200 ) ) ;
#6175 = ORIENTED_EDGE ( 'NONE', *, *, #10481, .F. ) ;
#6176 = VERTEX_POINT ( 'NONE', #16592 ) ;
#6177 = EDGE_CURVE ( 'NONE', #17454, #15773, #7803, .T. ) ;
#6178 = EDGE_CURVE ( 'NONE', #19406, #6147, #418, .T. ) ;
#6179 = CARTESIAN_POINT ( 'NONE',  ( 61.33076419740685736, 141.3451534613812441, 11.70407797152743079 ) ) ;
#6180 = ORIENTED_EDGE ( 'NONE', *, *, #1690, .T. ) ;
#6181 = CARTESIAN_POINT ( 'NONE',  ( 39.92123440845004723, 117.2344580088725792, 38.46393386101376421 ) ) ;
#6182 = CARTESIAN_POINT ( 'NONE',  ( 43.01140435219951286, 111.5344580088725905, 39.21067981925356349 ) ) ;
#6183 = AXIS2_PLACEMENT_3D ( 'NONE', #10596, #3980, #8731 ) ;
#6184 = CARTESIAN_POINT ( 'NONE',  ( 43.01140435219951286, 80.62977050742732388, 29.55568802177586463 ) ) ;
#6185 = CARTESIAN_POINT ( 'NONE',  ( 39.42975644700377558, 135.4151871740940010, 36.81289934271958941 ) ) ;
#6186 = CARTESIAN_POINT ( 'NONE',  ( 43.01140435219951286, 91.46049967264873715, 39.46799094044489209 ) ) ;
#6187 = CARTESIAN_POINT ( 'NONE',  ( 61.76154402333882132, 148.5480768402654803, 4.482004293238171400 ) ) ;
#6188 = CARTESIAN_POINT ( 'NONE',  ( 147.8787791192428074, -126.9891397928655010, 0.3429884183836981459 ) ) ;
#6189 = CARTESIAN_POINT ( 'NONE',  ( -157.6495955161842062, -161.9391397928654897, 41.15050349809590102 ) ) ;
#6190 = CARTESIAN_POINT ( 'NONE',  ( 38.58424406990784661, 87.26518717409399528, 35.64915139335016647 ) ) ;
#6191 = EDGE_CURVE ( 'NONE', #21705, #13430, #7912, .T. ) ;
#6192 = DIRECTION ( 'NONE',  ( 0.000000000000000000, 1.000000000000000000, 0.000000000000000000 ) ) ;
#6193 = CARTESIAN_POINT ( 'NONE',  ( 44.55648932407425633, 142.8844580088725991, 29.45539723777780239 ) ) ;
#6194 = ORIENTED_EDGE ( 'NONE', *, *, #2664, .T. ) ;
#6195 = CARTESIAN_POINT ( 'NONE',  ( 44.37947211624943833, 74.47977050742731819, 30.00020018409699318 ) ) ;
#6196 = CARTESIAN_POINT ( 'NONE',  ( -142.0420953463935803, -159.5438272943107449, 52.72008163687743831 ) ) ;
#6197 = CARTESIAN_POINT ( 'NONE',  ( 66.24914683137549787, 94.76885710642066840, 6.506024766557033878 ) ) ;
#6198 = CARTESIAN_POINT ( 'NONE',  ( -154.3824083646099439, -184.5584106276440650, 58.62277379824867296 ) ) ;
#6199 = AXIS2_PLACEMENT_3D ( 'NONE', #19835, #4616, #11337 ) ;
#6200 = ORIENTED_EDGE ( 'NONE', *, *, #929, .T. ) ;
#6201 = CARTESIAN_POINT ( 'NONE',  ( 147.5268905834513475, 193.0332408774651185, 4.000000000000021316 ) ) ;
#6202 = VECTOR ( 'NONE', #20458, 1000.000000000000227 ) ;
#6203 = CARTESIAN_POINT ( 'NONE',  ( 43.80332655382220253, 123.6113394311928317, 39.21067981925355639 ) ) ;
#6204 = CARTESIAN_POINT ( 'NONE',  ( 43.01140435219951286, 119.6297705074273097, 29.55568802177586107 ) ) ;
#6205 = ORIENTED_EDGE ( 'NONE', *, *, #17394, .F. ) ;
#6206 = SHAPE_REPRESENTATION ( 'Material Hold-Down Screw Clamp', ( #12657 ), #2455 ) ;
#6207 = CARTESIAN_POINT ( 'NONE',  ( 23.10700517764655260, 139.6571016847272801, -10.96257334342637435 ) ) ;
#6208 = EDGE_LOOP ( 'NONE', ( #11910, #13559, #15642, #3783 ) ) ;
#6209 = CARTESIAN_POINT ( 'NONE',  ( 45.74753988029933538, 124.4297705074273068, 37.97664729208901946 ) ) ;
#6210 = CARTESIAN_POINT ( 'NONE',  ( 38.01140435219952707, 72.86049967264874283, 35.83527830041809636 ) ) ;
#6211 = CARTESIAN_POINT ( 'NONE',  ( 38.01140435219952707, 65.78445800887257633, 34.21067981925357060 ) ) ;
#6212 = EDGE_CURVE ( 'NONE', #13667, #7226, #21179, .T. ) ;
#6213 = VECTOR ( 'NONE', #13361, 1000.000000000000000 ) ;
#6214 = DIRECTION ( 'NONE',  ( -1.000000000000000000, 0.000000000000000000, 0.000000000000000000 ) ) ;
#6215 = FACE_OUTER_BOUND ( 'NONE', #2651, .T. ) ;
#6216 = CARTESIAN_POINT ( 'NONE',  ( -141.4692556286852891, -186.8391397928654385, 46.40781461928724383 ) ) ;
#6217 = LINE ( 'NONE', #1594, #3452 ) ;
#6218 = CARTESIAN_POINT ( 'NONE',  ( 48.01140435219951996, 131.0604996726487457, 35.83527830041809636 ) ) ;
#6219 = CARTESIAN_POINT ( 'NONE',  ( -160.8964159109769696, -187.7438272943107336, 52.72008163687743121 ) ) ;
#6220 = APPLICATION_PROTOCOL_DEFINITION ( 'draft international standard', 'automotive_design', 1998, #12376 ) ;
#6221 = CARTESIAN_POINT ( 'NONE',  ( 47.05648932407426344, 124.5844580088725735, 31.27175355779120025 ) ) ;
#6222 = CARTESIAN_POINT ( 'NONE',  ( 41.64333658814960870, 99.97977050742731819, 38.42115945441014446 ) ) ;
#6223 = CARTESIAN_POINT ( 'NONE',  ( 51.94691807752363388, 146.6530262932614050, -9.724486432582017059 ) ) ;
#6224 = CARTESIAN_POINT ( 'NONE',  ( -160.8964159109769696, -181.7438272943107336, 52.72008163687743121 ) ) ;
#6225 = CARTESIAN_POINT ( 'NONE',  ( 38.58424406990786082, 99.11518717409400381, 34.21067981925357060 ) ) ;
#6226 = CARTESIAN_POINT ( 'NONE',  ( 38.01140435219952707, 84.86049967264872862, 35.83527830041809636 ) ) ;
#6227 = VERTEX_POINT ( 'NONE', #16375 ) ;
#6228 = FACE_BOUND ( 'NONE', #4406, .T. ) ;
#6229 = ADVANCED_FACE ( 'NONE', ( #16482, #4585, #11305 ), #6355, .F. ) ;
#6230 = CARTESIAN_POINT ( 'NONE',  ( 66.76198117565915879, 95.25264312590786631, -0.5179092472497510702 ) ) ;
#6231 = CARTESIAN_POINT ( 'NONE',  ( 64.82873087846098770, 102.1656695083886603, -13.57732884656604355 ) ) ;
#6232 = CARTESIAN_POINT ( 'NONE',  ( 43.01140435219951286, 68.62977050742729546, 29.55568802177586107 ) ) ;
#6233 =( BOUNDED_CURVE ( )  B_SPLINE_CURVE ( 2, ( #1087, #4380, #4712, #21153, #14630, #17931, #12989, #8036, #1414, #6038, #11112, #11215, #4824 ),
 .UNSPECIFIED., .F., .F. ) 
 B_SPLINE_CURVE_WITH_KNOTS ( ( 3, 2, 2, 2, 2, 2, 3 ),
 ( 0.7426470588235294379, 0.7441176470588235503, 0.7470588235294117752, 0.7500000000000000000, 0.7529411764705882248, 0.7558823529411764497, 0.7573529411764705621 ),
 .UNSPECIFIED. ) 
 CURVE ( )  GEOMETRIC_REPRESENTATION_ITEM ( )  RATIONAL_B_SPLINE_CURVE ( ( 0.9755282581475768211, 0.9755282581475768211, 1.000000000000000000, 0.9510565162951535312, 1.000000000000000000, 0.9510565162951535312, 1.000000000000000000, 0.9510565162951535312, 1.000000000000000000, 0.9510565162951535312, 1.000000000000000000, 0.9755282581475768211, 0.9755282581475768211 ) ) 
 REPRESENTATION_ITEM ( '' )  );
#6234 = ORIENTED_EDGE ( 'NONE', *, *, #1158, .F. ) ;
#6235 = EDGE_CURVE ( 'NONE', #8905, #7289, #13727, .T. ) ;
#6236 = ORIENTED_EDGE ( 'NONE', *, *, #14985, .F. ) ;
#6237 = CARTESIAN_POINT ( 'NONE',  ( 38.58424406990786082, 156.3797705074273097, 34.21067981925357060 ) ) ;
#6238 = CARTESIAN_POINT ( 'NONE',  ( 0.000000000000000000, -37.13255853780189852, 30.00000000000000000 ) ) ;
#6239 = AXIS2_PLACEMENT_3D ( 'NONE', #4196, #354, #18974 ) ;
#6240 = CARTESIAN_POINT ( 'NONE',  ( 39.92123440845004723, 109.1604996726487542, 38.46393386101376421 ) ) ;
#6241 = CARTESIAN_POINT ( 'NONE',  ( 46.59305225739526435, 64.31518717409399244, 36.81289934271958941 ) ) ;
#6242 = CARTESIAN_POINT ( 'NONE',  ( 39.92123440845005433, 65.33445800887258770, 29.95742577749336988 ) ) ;
#6243 = CARTESIAN_POINT ( 'NONE',  ( -154.3824083646099439, -164.4938272943107336, 40.69124936498395328 ) ) ;
#6244 = VECTOR ( 'NONE', #11505, 1000.000000000000000 ) ;
#6245 = LINE ( 'NONE', #6357, #17773 ) ;
#6246 = CARTESIAN_POINT ( 'NONE',  ( -148.3790856849358306, -176.4630981290893033, 40.14644641866477315 ) ) ;
#6247 = CARTESIAN_POINT ( 'NONE',  ( -151.4692556286852891, -196.9891397928655010, 39.65701158161630246 ) ) ;
#6248 = CARTESIAN_POINT ( 'NONE',  ( 43.01140435219951286, 152.0344580088725763, 28.95336869806222779 ) ) ;
#6249 = CARTESIAN_POINT ( 'NONE',  ( 45.74753988029933538, 136.4297705074273210, 37.97664729208901946 ) ) ;
#6250 = CARTESIAN_POINT ( 'NONE',  ( 8.804574439154260190, 117.1883747968346654, 15.00137004459121393 ) ) ;
#6251 = CARTESIAN_POINT ( 'NONE',  ( 44.37947211624943833, 127.0151871740939953, 38.42115945441014446 ) ) ;
#6252 = CARTESIAN_POINT ( 'NONE',  ( -157.6495955161842062, -167.0391397928654555, 58.16351966513671812 ) ) ;
#6253 = CARTESIAN_POINT ( 'NONE',  ( -148.5561028927606344, -160.2584106276440536, 58.62277379824867296 ) ) ;
#6254 = DIRECTION ( 'NONE',  ( 0.4874675571821264763, 0.8731411001063288380, 0.000000000000000000 ) ) ;
#6255 = LINE ( 'NONE', #17714, #19428 ) ;
#6256 = CARTESIAN_POINT ( 'NONE',  ( 58.35211712195835076, 96.24552883246097679, -7.224606741634919338 ) ) ;
#6257 = VECTOR ( 'NONE', #7033, 1000.000000000000000 ) ;
#6258 = CARTESIAN_POINT ( 'NONE',  ( 42.21948215057684450, 120.0373810949690210, 29.21067981925356705 ) ) ;
#6259 = ORIENTED_EDGE ( 'NONE', *, *, #16877, .T. ) ;
#6260 = DIRECTION ( 'NONE',  ( -0.000000000000000000, -0.000000000000000000, 1.000000000000000000 ) ) ;
#6261 = ORIENTED_EDGE ( 'NONE', *, *, #1857, .T. ) ;
#6262 = CARTESIAN_POINT ( 'NONE',  ( 43.01140435219951286, 83.03445800887257633, 28.95336869806222779 ) ) ;
#6263 = CARTESIAN_POINT ( 'NONE',  ( -79.69854755000110913, 605.3054376597395958, -3.999999999999980904 ) ) ;
#6264 = CARTESIAN_POINT ( 'NONE',  ( 38.96631938032478359, 136.0104996726487627, 37.14960608071593384 ) ) ;
#6266 = CARTESIAN_POINT ( 'NONE',  ( 36.80677928932056631, 92.47987693618573246, 1.660900796654692702 ) ) ;
#6265 = CARTESIAN_POINT ( 'NONE',  ( 41.64333658814960870, 98.51518717409399528, 30.00020018409699318 ) ) ;
#6267 = DIRECTION ( 'NONE',  ( 0.000000000000000000, -1.000000000000000000, 0.000000000000000000 ) ) ;
#6268 = EDGE_CURVE ( 'NONE', #17720, #10563, #10329, .T. ) ;
#6269 = CARTESIAN_POINT ( 'NONE',  ( -142.0420953463935803, -171.5084106276440536, 46.59394152635518793 ) ) ;
#6270 = CARTESIAN_POINT ( 'NONE',  ( 47.05648932407426344, 64.91049967264873999, 37.14960608071593384 ) ) ;
#6272 = DIRECTION ( 'NONE',  ( -0.000000000000000000, -0.000000000000000000, 1.000000000000000000 ) ) ;
#6271 = CARTESIAN_POINT ( 'NONE',  ( 43.01140435219951286, 127.4604996726487229, 39.21067981925356349 ) ) ;
#6273 = CARTESIAN_POINT ( 'NONE',  ( -148.3790856849358306, -188.4630981290893317, 40.14644641866477315 ) ) ;
#6274 = CYLINDRICAL_SURFACE ( 'NONE', #9672, 16.96660865288809816 ) ;
#6275 = CARTESIAN_POINT ( 'NONE',  ( 43.01140435219951286, 116.0344580088725763, 29.21067981925356705 ) ) ;
#6276 = CARTESIAN_POINT ( 'NONE',  ( 40.27526882409969033, 156.8297705074272983, 37.97664729208901946 ) ) ;
#6277 = CARTESIAN_POINT ( 'NONE',  ( 74.62708615766334219, 133.0342049366344384, -8.851289726714327344 ) ) ;
#6278 = DIRECTION ( 'NONE',  ( 0.000000000000000000, 1.000000000000000000, 0.000000000000000000 ) ) ;
#6279 = CARTESIAN_POINT ( 'NONE',  ( -154.3824083646099439, -169.2938272943107165, 58.62277379824867296 ) ) ;
#6280 = CARTESIAN_POINT ( 'NONE',  ( -145.6429501568359797, -187.1084106276440480, 57.67623309621197336 ) ) ;
#6281 = EDGE_CURVE ( 'NONE', #8122, #12991, #10294, .T. ) ;
#6282 = ADVANCED_FACE ( 'NONE', ( #12072 ), #11862, .T. ) ;
#6283 = ORIENTED_EDGE ( 'NONE', *, *, #16598, .F. ) ;
#6284 = CARTESIAN_POINT ( 'NONE',  ( 47.43856463449117911, 73.46518717409398391, 35.64915139335015937 ) ) ;
#6285 = CARTESIAN_POINT ( 'NONE',  ( -151.4692556286852891, -164.9084106276440593, 39.74470866294723947 ) ) ;
#6286 = CARTESIAN_POINT ( 'NONE',  ( 9.955767346236717330, 110.6995739201198887, 21.78706596723887756 ) ) ;
#6287 = CARTESIAN_POINT ( 'NONE',  ( 43.80332655382220253, 111.6113394311928317, 39.21067981925355639 ) ) ;
#6288 = CARTESIAN_POINT ( 'NONE',  ( 43.01140435219951286, 132.8651871740940180, 38.86567161673127657 ) ) ;
#6289 = CARTESIAN_POINT ( 'NONE',  ( 13.96574040630659752, 137.8735611475157157, -3.299202782472894224 ) ) ;
#6290 = ORIENTED_EDGE ( 'NONE', *, *, #8145, .F. ) ;
#6291 = ORIENTED_EDGE ( 'NONE', *, *, #8119, .F. ) ;
#6292 = CARTESIAN_POINT ( 'NONE',  ( 68.77576173894735234, 108.4446202281264249, 13.13264940013829296 ) ) ;
#6293 = VERTEX_POINT ( 'NONE', #8348 ) ;
#6294 = EDGE_CURVE ( 'NONE', #8663, #19941, #10437, .T. ) ;
#6295 = DIRECTION ( 'NONE',  ( -0.000000000000000000, 1.000000000000000000, -0.000000000000000000 ) ) ;
#6296 = CIRCLE ( 'NONE', #14048, 21.90454335994854063 ) ;
#6297 = CARTESIAN_POINT ( 'NONE',  ( 47.43856463449117200, 74.02977050742730114, 32.77220824515698183 ) ) ;
#6299 = CARTESIAN_POINT ( 'NONE',  ( 71.19791805076843616, 120.7596060772701776, 5.632536115698772328 ) ) ;
#6298 = CARTESIAN_POINT ( 'NONE',  ( 39.42975644700377558, 129.4151871740940010, 36.81289934271958941 ) ) ;
#6300 =( BOUNDED_CURVE ( )  B_SPLINE_CURVE ( 2, ( #16711, #18145, #21580, #1620, #11752, #6471, #1733, #8468, #8352, #3053, #8243, #21800, #9896 ),
 .UNSPECIFIED., .F., .F. ) 
 B_SPLINE_CURVE_WITH_KNOTS ( ( 3, 2, 2, 2, 2, 2, 3 ),
 ( 0.4632352941176470784, 0.4647058823529411908, 0.4676470588235294157, 0.4705882352941176405, 0.4735294117647058654, 0.4764705882352940902, 0.4779411764705882582 ),
 .UNSPECIFIED. ) 
 CURVE ( )  GEOMETRIC_REPRESENTATION_ITEM ( )  RATIONAL_B_SPLINE_CURVE ( ( 0.9755282581475768211, 0.9755282581475768211, 1.000000000000000000, 0.9510565162951535312, 1.000000000000000000, 0.9510565162951535312, 1.000000000000000000, 0.9510565162951535312, 1.000000000000000000, 0.9510565162951535312, 1.000000000000000000, 0.9755282581475763770, 0.9755282581475768211 ) ) 
 REPRESENTATION_ITEM ( '' )  );
#6301 = CARTESIAN_POINT ( 'NONE',  ( 46.10157429594899270, 95.66049967264871157, 29.95742577749337343 ) ) ;
#6302 = CARTESIAN_POINT ( 'NONE',  ( 74.27779736592162863, 105.9683817680885056, 13.05343286460986363 ) ) ;
#6303 = CARTESIAN_POINT ( 'NONE',  ( 43.01140435219951286, 59.96049967264874425, 29.21067981925356705 ) ) ;
#6304 = CARTESIAN_POINT ( 'NONE',  ( -141.4692556286852891, -162.9891397928654726, 49.65701158161630957 ) ) ;
#6305 = CARTESIAN_POINT ( 'NONE',  ( 45.74753988029933538, 91.16518717409397254, 37.97664729208901946 ) ) ;
#6306 = ADVANCED_FACE ( 'NONE', ( #6705 ), #3943, .T. ) ;
#6307 = CARTESIAN_POINT ( 'NONE',  ( 41.39629556124358345, 144.8566973352396587, 38.95396702123350252 ) ) ;
#6308 = CARTESIAN_POINT ( 'NONE',  ( 46.10157429594899270, 71.66049967264873999, 29.95742577749336988 ) ) ;
#6309 = CARTESIAN_POINT ( 'NONE',  ( -154.5594255724347761, -186.0891397928654953, 40.14644641866476604 ) ) ;
#6310 = EDGE_LOOP ( 'NONE', ( #2393, #604 ) ) ;
#6311 = CARTESIAN_POINT ( 'NONE',  ( 41.64333658814960870, 75.97977050742731819, 38.42115945441014446 ) ) ;
#6312 = CARTESIAN_POINT ( 'NONE',  ( -159.0959885057557983, -193.8584106276440480, 55.19815736654470584 ) ) ;
#6313 = CARTESIAN_POINT ( 'NONE',  ( 13.78455932396994577, 137.7305411390292420, 2.696406107442721467 ) ) ;
#6314 = CARTESIAN_POINT ( 'NONE',  ( -160.8964159109769696, -182.3084106276440650, 46.59394152635518793 ) ) ;
#6315 = ORIENTED_EDGE ( 'NONE', *, *, #20512, .T. ) ;
#6316 = CARTESIAN_POINT ( 'NONE',  ( 41.64333658814960870, 158.5151871740940237, 30.00020018409699318 ) ) ;
#6317 = AXIS2_PLACEMENT_3D ( 'NONE', #2688, #17781, #7779 ) ;
#6318 = CARTESIAN_POINT ( 'NONE',  ( -141.4692556286852891, -160.1391397928654499, 52.90620854394536821 ) ) ;
#6319 = CARTESIAN_POINT ( 'NONE',  ( 45.74753988029934249, 124.4297705074273210, 37.97664729208901235 ) ) ;
#6320 = VERTEX_POINT ( 'NONE', #5143 ) ;
#6321 = EDGE_LOOP ( 'NONE', ( #2363, #3372, #15985, #5189 ) ) ;
#6322 = CARTESIAN_POINT ( 'NONE',  ( 47.43856463449118621, 118.8797705074273239, 34.21067981925357060 ) ) ;
#6323 = CARTESIAN_POINT ( 'NONE',  ( 43.01140435219951286, 130.4604996726487229, 39.21067981925356349 ) ) ;
#6324 = CARTESIAN_POINT ( 'NONE',  ( 40.27526882409969033, 89.92977050742730682, 30.44471234641811819 ) ) ;
#6325 = CARTESIAN_POINT ( 'NONE',  ( 48.01140435219951996, 67.43445800887256780, 32.58608133808903773 ) ) ;
#6326 = PRODUCT_DEFINITION_FORMATION_WITH_SPECIFIED_SOURCE ( 'ANY', '', #6562, .NOT_KNOWN. ) ;
#6327 = DIRECTION ( 'NONE',  ( 0.3428981916074309577, -0.9393725726208709270, 0.000000000000000000 ) ) ;
#6328 = DIRECTION ( 'NONE',  ( 0.000000000000000000, 1.000000000000000000, 0.000000000000000000 ) ) ;
#6329 = SURFACE_SIDE_STYLE ('',( #14808 ) ) ;
#6330 = CARTESIAN_POINT ( 'NONE',  ( -141.4692556286852891, -190.1391397928655067, 52.90620854394536821 ) ) ;
#6331 = DIRECTION ( 'NONE',  ( -1.000000000000000000, 0.000000000000000000, 0.000000000000000000 ) ) ;
#6332 = CARTESIAN_POINT ( 'NONE',  ( 38.96631938032478359, 102.4104996726487400, 31.27175355779120025 ) ) ;
#6333 = CARTESIAN_POINT ( 'NONE',  ( -145.6429501568359797, -192.8438272943107563, 57.67623309621198047 ) ) ;
#6334 = CONTEXT_DEPENDENT_SHAPE_REPRESENTATION ( #5908, #18206 ) ;
#6335 = CARTESIAN_POINT ( 'NONE',  ( 41.46631938032478359, 119.1844580088725962, 29.45539723777780239 ) ) ;
#6336 = CARTESIAN_POINT ( 'NONE',  ( 46.59305225739526435, 103.5797705074273267, 36.81289934271958941 ) ) ;
#6337 = CARTESIAN_POINT ( 'NONE',  ( 21.79768317403592803, 101.2052074350461339, 14.36631359211887649 ) ) ;
#6338 = CARTESIAN_POINT ( 'NONE',  ( -151.4692556286852891, -181.1438272943107393, 59.56931450028537967 ) ) ;
#6339 = CARTESIAN_POINT ( 'NONE',  ( 41.64333658814960870, 87.71518717409399812, 38.42115945441014446 ) ) ;
#6340 = DIRECTION ( 'NONE',  ( 0.000000000000000000, 1.000000000000000000, 0.000000000000000000 ) ) ;
#6341 = VERTEX_POINT ( 'NONE', #292 ) ;
#6342 = FACE_OUTER_BOUND ( 'NONE', #21079, .T. ) ;
#6343 = CARTESIAN_POINT ( 'NONE',  ( 73.40451243997107156, 135.6611253642151098, -1.946480675884423084 ) ) ;
#6344 = CARTESIAN_POINT ( 'NONE',  ( 49.88381083390898851, 92.64041853056629350, -12.86295667411130239 ) ) ;
#6345 = AXIS2_PLACEMENT_3D ( 'NONE', #6171, #4631, #11458 ) ;
#6346 = CARTESIAN_POINT ( 'NONE',  ( 44.37947211624943833, 71.47977050742731819, 30.00020018409699318 ) ) ;
#6347 = ORIENTED_EDGE ( 'NONE', *, *, #2520, .F. ) ;
#6348 = ORIENTED_EDGE ( 'NONE', *, *, #6001, .T. ) ;
#6349 = CARTESIAN_POINT ( 'NONE',  ( 43.01140435219951286, 155.6297705074273381, 29.55568802177586463 ) ) ;
#6350 = EDGE_CURVE ( 'NONE', #17423, #19975, #18376, .T. ) ;
#6351 = EDGE_CURVE ( 'NONE', #21430, #2361, #11676, .T. ) ;
#6352 = CARTESIAN_POINT ( 'NONE',  ( -151.4692556286852891, -126.9891397928655010, 59.65701158161632378 ) ) ;
#6353 = CARTESIAN_POINT ( 'NONE',  ( 46.10157429594899270, 106.7604996726487201, 38.46393386101376421 ) ) ;
#6354 = CARTESIAN_POINT ( 'NONE',  ( 40.27526882409969033, 72.56518717409399244, 37.97664729208901946 ) ) ;
#6355 = PLANE ( 'NONE',  #3238 ) ;
#6356 = CARTESIAN_POINT ( 'NONE',  ( -151.4692556286852891, -160.1438272943107393, 59.56931450028537256 ) ) ;
#6357 = CARTESIAN_POINT ( 'NONE',  ( 43.01140435219951996, 10.71049967264875491, 29.21067981925357060 ) ) ;
#6358 = CARTESIAN_POINT ( 'NONE',  ( -141.4692556286852891, -174.2130981290893033, 52.90620854394536821 ) ) ;
#6359 = AXIS2_PLACEMENT_3D ( 'NONE', #21368, #1302, #9582 ) ;
#6360 = CARTESIAN_POINT ( 'NONE',  ( -120.0322075325610598, -126.9891397928655010, -34.99999999999999289 ) ) ;
#6361 = CARTESIAN_POINT ( 'NONE',  ( 39.92123440845004723, 152.3344580088725593, 29.95742577749337343 ) ) ;
#6362 = CARTESIAN_POINT ( 'NONE',  ( 47.43856463449117200, 130.7297705074273040, 35.64915139335016647 ) ) ;
#6363 = CARTESIAN_POINT ( 'NONE',  ( 58.41865009756546812, 150.5677012977470781, 10.35848337793017393 ) ) ;
#6364 = CARTESIAN_POINT ( 'NONE',  ( 46.59305225739526435, 115.9151871740940010, 31.60846029578754468 ) ) ;
#6365 = CARTESIAN_POINT ( 'NONE',  ( 111.4021762516569964, 137.5714195593754710, 4.000000000000021316 ) ) ;
#6366 = CARTESIAN_POINT ( 'NONE',  ( 38.01140435219952707, 150.7104996726487514, 34.21067981925357060 ) ) ;
#6367 = CARTESIAN_POINT ( 'NONE',  ( 131.4397495910615135, 111.2323268066561894, 4.000000000000021316 ) ) ;
#6368 = DIRECTION ( 'NONE',  ( 0.000000000000000000, 0.000000000000000000, 1.000000000000000000 ) ) ;
#6369 = CARTESIAN_POINT ( 'NONE',  ( 64.05606230151549596, 101.0139342820504993, 19.48556066606253978 ) ) ;
#6370 = DIRECTION ( 'NONE',  ( 0.000000000000000000, 1.000000000000000000, 0.000000000000000000 ) ) ;
#6371 = ORIENTED_EDGE ( 'NONE', *, *, #19690, .F. ) ;
#6372 = DIRECTION ( 'NONE',  ( -1.000000000000000000, 0.000000000000000000, -0.000000000000000000 ) ) ;
#6373 = ORIENTED_EDGE ( 'NONE', *, *, #19599, .T. ) ;
#6374 = CARTESIAN_POINT ( 'NONE',  ( 43.01140435219951286, 80.03445800887256212, 28.95336869806222779 ) ) ;
#6375 = CARTESIAN_POINT ( 'NONE',  ( 173.3794444120442506, -37.13255853780189852, 30.00000000000000000 ) ) ;
#6376 = CARTESIAN_POINT ( 'NONE',  ( 38.01140435219952707, 138.7104996726487514, 34.21067981925357060 ) ) ;
#6378 = CARTESIAN_POINT ( 'NONE',  ( 59.14563986918259531, 96.87627350248034475, 7.732070471200789719 ) ) ;
#6377 = CARTESIAN_POINT ( 'NONE',  ( 38.58424406990784661, 92.96518717409401233, 32.77220824515698183 ) ) ;
#6379 = LINE ( 'NONE', #13108, #20764 ) ;
#6380 = CARTESIAN_POINT ( 'NONE',  ( -142.0420953463935803, -168.8084106276440650, 52.72008163687743831 ) ) ;
#6381 = CARTESIAN_POINT ( 'NONE',  ( -145.6429501568359797, -192.8438272943107279, 57.67623309621197336 ) ) ;
#6383 = CARTESIAN_POINT ( 'NONE',  ( -136.6255475934131596, 760.1741454933652449, -3.999999999999980904 ) ) ;
#6382 = LINE ( 'NONE', #13112, #4461 ) ;
#6384 = LINE ( 'NONE', #4617, #15109 ) ;
#6385 = EDGE_CURVE ( 'NONE', #12631, #21815, #15059, .T. ) ;
#6386 = CARTESIAN_POINT ( 'NONE',  ( 43.01140435219951996, 10.71049967264875491, 39.21067981925356349 ) ) ;
#6387 = LINE ( 'NONE', #1760, #2740 ) ;
#6388 = CARTESIAN_POINT ( 'NONE',  ( 38.58424406990786082, 60.11518717409400381, 34.21067981925357060 ) ) ;
#6389 = CARTESIAN_POINT ( 'NONE',  ( 39.92123440845005433, 153.2344580088725934, 38.46393386101375711 ) ) ;
#6390 = ADVANCED_FACE ( 'NONE', ( #3605, #5039, #17031 ), #6811, .T. ) ;
#6391 = CARTESIAN_POINT ( 'NONE',  ( 9.021810916323596885, 123.9851095102452945, 2.220310480865780534 ) ) ;
#6392 = CARTESIAN_POINT ( 'NONE',  ( -151.4692556286852891, -160.1438272943107393, 59.56931450028537967 ) ) ;
#6393 = CARTESIAN_POINT ( 'NONE',  ( -159.0959885057557983, -182.4584106276440707, 44.11586579668791330 ) ) ;
#6394 = VERTEX_POINT ( 'NONE', #3498 ) ;
#6395 = CARTESIAN_POINT ( 'NONE',  ( 45.74753988029934249, 70.16518717409397254, 37.97664729208901235 ) ) ;
#6396 = CARTESIAN_POINT ( 'NONE',  ( -148.5561028927606344, -172.2584106276440536, 58.62277379824867296 ) ) ;
#6397 = CARTESIAN_POINT ( 'NONE',  ( 49.69400319086401652, 86.25038505451357196, 20.12058643263999969 ) ) ;
#6398 = CARTESIAN_POINT ( 'NONE',  ( 173.3794444120442506, -84.13255853780189852, 5.000000000000018652 ) ) ;
#6399 = CARTESIAN_POINT ( 'NONE',  ( 46.59305225739526435, 130.3151871740940067, 36.81289934271958941 ) ) ;
#6400 = CARTESIAN_POINT ( 'NONE',  ( 9.783399875253829592, 127.8057224500684015, -3.656374068424393275 ) ) ;
#6401 = ORIENTED_EDGE ( 'NONE', *, *, #2476, .T. ) ;
#6402 = EDGE_LOOP ( 'NONE', ( #847, #658 ) ) ;
#6403 = VECTOR ( 'NONE', #10949, 1000.000000000000114 ) ;
#6404 = VECTOR ( 'NONE', #17203, 1000.000000000000000 ) ;
#6405 = CARTESIAN_POINT ( 'NONE',  ( 16.70103016558074316, 129.9804388327498827, 16.57432765154378629 ) ) ;
#6406 = VERTEX_POINT ( 'NONE', #18480 ) ;
#6407 = CARTESIAN_POINT ( 'NONE',  ( 43.01140435219951286, 110.0344580088725621, 28.95336869806222779 ) ) ;
#6408 = LINE ( 'NONE', #8183, #19940 ) ;
#6409 = AXIS2_PLACEMENT_3D ( 'NONE', #13412, #20146, #400 ) ;
#6410 = ADVANCED_FACE ( 'NONE', ( #18700 ), #18369, .T. ) ;
#6411 = CARTESIAN_POINT ( 'NONE',  ( 39.42975644700377558, 63.07977050742731251, 31.60846029578754468 ) ) ;
#6413 = CARTESIAN_POINT ( 'NONE',  ( 42.95897134029118547, 91.70801217734280897, 7.418363685804686192 ) ) ;
#6412 = CARTESIAN_POINT ( 'NONE',  ( 40.27526882409969033, 129.5651871740940067, 37.97664729208901946 ) ) ;
#6414 = CARTESIAN_POINT ( 'NONE',  ( 44.55648932407425633, 83.81049967264874567, 29.45539723777780239 ) ) ;
#6415 = CARTESIAN_POINT ( 'NONE',  ( 180.1254907973641934, 54.87273858953557237, -19.99999999999997868 ) ) ;
#6416 = CARTESIAN_POINT ( 'NONE',  ( -149.8854112254399240, -170.3899795514095672, 39.65701158161629536 ) ) ;
#6417 = CYLINDRICAL_SURFACE ( 'NONE', #6993, 10.00000000000000888 ) ;
#6418 = CARTESIAN_POINT ( 'NONE',  ( 38.58424406990784661, 89.96518717409399812, 32.77220824515698183 ) ) ;
#6419 = PRODUCT ( 'Handle Grip', 'Handle Grip', '', ( #19556 ) ) ;
#6420 = COLOUR_RGB ( '', 0.72549020, 0.75294118, 0.79215686) ;
#6421 = CARTESIAN_POINT ( 'NONE',  ( -154.5594255724347761, -184.8891397928654783, 59.16757674456785310 ) ) ;
#6422 = VERTEX_POINT ( 'NONE', #8674 ) ;
#6423 = CARTESIAN_POINT ( 'NONE',  ( 40.27526882409969033, 68.92977050742733525, 30.44471234641811819 ) ) ;
#6424 = CARTESIAN_POINT ( 'NONE',  ( -148.5561028927606344, -193.2584106276440252, 58.62277379824867296 ) ) ;
#6425 = CARTESIAN_POINT ( 'NONE',  ( 25.52397925108762067, 90.47728371212039633, 7.934596195134201224 ) ) ;
#6426 = CARTESIAN_POINT ( 'NONE',  ( -145.6429501568359797, -189.2084106276440423, 41.63779006702063867 ) ) ;
#6427 = ORIENTED_EDGE ( 'NONE', *, *, #9863, .F. ) ;
#6428 = CARTESIAN_POINT ( 'NONE',  ( -161.4692556286852891, -161.6391397928654783, 46.40781461928724383 ) ) ;
#6429 = CARTESIAN_POINT ( 'NONE',  ( -151.4692556286852607, -160.7391397928654158, 59.65701158161632378 ) ) ;
#6430 = CARTESIAN_POINT ( 'NONE',  ( 43.01140435219951286, 125.6297705074273381, 29.55568802177586107 ) ) ;
#6431 = VERTEX_POINT ( 'NONE', #8569 ) ;
#6432 = CARTESIAN_POINT ( 'NONE',  ( 43.01140435219951996, 158.0344580088725763, 29.21067981925357060 ) ) ;
#6433 =( BOUNDED_CURVE ( )  B_SPLINE_CURVE ( 2, ( #13972, #15427, #2190, #8921, #17385, #20710, #7053, #322, #20602, #8708, #13544, #18622, #12103 ),
 .UNSPECIFIED., .F., .F. ) 
 B_SPLINE_CURVE_WITH_KNOTS ( ( 3, 2, 2, 2, 2, 2, 3 ),
 ( 0.1544117647058823595, 0.1558823529411764719, 0.1588235294117646967, 0.1617647058823529493, 0.1647058823529411742, 0.1676470588235293990, 0.1691176470588235115 ),
 .UNSPECIFIED. ) 
 CURVE ( )  GEOMETRIC_REPRESENTATION_ITEM ( )  RATIONAL_B_SPLINE_CURVE ( ( 0.9755282581475768211, 0.9755282581475768211, 1.000000000000000000, 0.9510565162951535312, 1.000000000000000000, 0.9510565162951535312, 1.000000000000000000, 0.9510565162951535312, 1.000000000000000000, 0.9510565162951535312, 1.000000000000000000, 0.9755282581475769321, 0.9755282581475765991 ) ) 
 REPRESENTATION_ITEM ( '' )  );
#6434 = ORIENTED_EDGE ( 'NONE', *, *, #12395, .F. ) ;
#6435 = CARTESIAN_POINT ( 'NONE',  ( 40.27526882409969033, 119.9297705074272926, 30.44471234641811819 ) ) ;
#6436 = CARTESIAN_POINT ( 'NONE',  ( 38.01140435219952707, 72.56049967264874567, 32.58608133808903773 ) ) ;
#6437 = EDGE_CURVE ( 'NONE', #8301, #18099, #15396, .T. ) ;
#6438 = CARTESIAN_POINT ( 'NONE',  ( 38.58424406990786082, 150.1151871740939896, 34.21067981925357060 ) ) ;
#6439 = CARTESIAN_POINT ( 'NONE',  ( 147.5268905834513475, 193.0332408774651185, 14.00000000000001776 ) ) ;
#6440 = CARTESIAN_POINT ( 'NONE',  ( 38.01140435219952707, 83.93445800887256780, 35.83527830041809636 ) ) ;
#6441 = CARTESIAN_POINT ( 'NONE',  ( 39.92123440845005433, 96.26049967264876273, 29.95742577749336988 ) ) ;
#6442 = CARTESIAN_POINT ( 'NONE',  ( -141.4692556286852891, -177.9891397928654442, 49.65701158161630957 ) ) ;
#6443 = LINE ( 'NONE', #4785, #6244 ) ;
#6444 = CARTESIAN_POINT ( 'NONE',  ( 46.10157429594899270, 130.7604996726487343, 38.46393386101375711 ) ) ;
#6445 = CARTESIAN_POINT ( 'NONE',  ( -143.8425227516148084, -186.6938272943107222, 55.19815736654470584 ) ) ;
#6446 = SHAPE_DEFINITION_REPRESENTATION ( #4284, #15921 ) ;
#6447 = CARTESIAN_POINT ( 'NONE',  ( 46.10157429594899270, 127.7344580088725792, 29.95742577749337343 ) ) ;
#6448 = CARTESIAN_POINT ( 'NONE',  ( 44.37947211624943833, 106.2797705074273154, 38.42115945441014446 ) ) ;
#6449 = CARTESIAN_POINT ( 'NONE',  ( 14.76087776054169787, 121.2312262212812755, 22.22355758277721804 ) ) ;
#6450 = CARTESIAN_POINT ( 'NONE',  ( -160.8964159109769696, -188.0438272943107449, 46.59394152635518793 ) ) ;
#6451 = CARTESIAN_POINT ( 'NONE',  ( 41.64333658814960870, 84.71518717409399812, 38.42115945441014446 ) ) ;
#6452 = CARTESIAN_POINT ( 'NONE',  ( 43.01140435219951286, 89.96049967264873715, 29.21067981925356705 ) ) ;
#6453 = VERTEX_POINT ( 'NONE', #16707 ) ;
#6454 = DIRECTION ( 'NONE',  ( -0.000000000000000000, -0.000000000000000000, -1.000000000000000000 ) ) ;
#6455 = CYLINDRICAL_SURFACE ( 'NONE', #4638, 27.14138364107347812 ) ;
#6456 = CARTESIAN_POINT ( 'NONE',  ( 39.42975644700377558, 144.0797705074273267, 31.60846029578754468 ) ) ;
#6457 = CARTESIAN_POINT ( 'NONE',  ( 42.74273477336613780, 91.78896094402264794, 1.422757611514577247 ) ) ;
#6458 = CARTESIAN_POINT ( 'NONE',  ( 41.64333658814960870, 71.77977050742731535, 30.00020018409699318 ) ) ;
#6459 = ORIENTED_EDGE ( 'NONE', *, *, #9404, .F. ) ;
#6460 = ORIENTED_EDGE ( 'NONE', *, *, #9801, .F. ) ;
#6461 = CARTESIAN_POINT ( 'NONE',  ( 40.27526882409969033, 147.8297705074272983, 37.97664729208901946 ) ) ;
#6462 = EDGE_CURVE ( 'NONE', #19662, #10404, #12153, .T. ) ;
#6463 = CARTESIAN_POINT ( 'NONE',  ( 138.4989748031516967, 208.9305787985672680, -29.99999999999997868 ) ) ;
#6464 = CARTESIAN_POINT ( 'NONE',  ( 38.01140435219951996, 108.5604996726487599, 32.58608133808903773 ) ) ;
#6465 = CARTESIAN_POINT ( 'NONE',  ( 40.27526882409969033, 71.66518717409400097, 30.44471234641811819 ) ) ;
#6466 = CARTESIAN_POINT ( 'NONE',  ( 38.01140435219952707, 95.63445800887255643, 32.58608133808903773 ) ) ;
#6467 = CARTESIAN_POINT ( 'NONE',  ( -148.5561028927606344, -159.9938272943107336, 58.62277379824867296 ) ) ;
#6468 = CARTESIAN_POINT ( 'NONE',  ( 39.92123440845005433, 156.2344580088725934, 38.46393386101375711 ) ) ;
#6469 = CARTESIAN_POINT ( 'NONE',  ( -143.3790856849358306, -182.7630981290893146, 43.77915905869157598 ) ) ;
#6470 =( NAMED_UNIT ( * ) SI_UNIT ( $, .STERADIAN. ) SOLID_ANGLE_UNIT ( ) );
#6471 = CARTESIAN_POINT ( 'NONE',  ( 38.01140435219952707, 111.8604996726487428, 35.83527830041809636 ) ) ;
#6472 = CARTESIAN_POINT ( 'NONE',  ( 48.01140435219951996, 151.1344580088726275, 35.83527830041810347 ) ) ;
#6473 = CARTESIAN_POINT ( 'NONE',  ( 40.27526882409969033, 131.9297705074273210, 30.44471234641811819 ) ) ;
#6474 = CARTESIAN_POINT ( 'NONE',  ( 8.710246811478747020, 120.8788544656517274, 15.12029029225770316 ) ) ;
#6475 = CARTESIAN_POINT ( 'NONE',  ( 38.58424406990785371, 116.9651871740939839, 32.77220824515697473 ) ) ;
#6476 = CARTESIAN_POINT ( 'NONE',  ( -151.4692556286852891, -181.7391397928654726, 59.65701158161631668 ) ) ;
#6477 = CIRCLE ( 'NONE', #1898, 27.58651506682278765 ) ;
#6478 = CARTESIAN_POINT ( 'NONE',  ( 43.01140435219951996, 10.71049967264875491, 29.21067981925357060 ) ) ;
#6479 = FACE_BOUND ( 'NONE', #21784, .T. ) ;
#6480 = CARTESIAN_POINT ( 'NONE',  ( 56.11190468687431832, 151.4478768383145280, 5.272225788895710252 ) ) ;
#6481 = CARTESIAN_POINT ( 'NONE',  ( 71.28758990370504023, 120.3962046462169440, 18.65202787790538608 ) ) ;
#6482 = DIRECTION ( 'NONE',  ( -0.000000000000000000, 1.000000000000000000, -0.000000000000000000 ) ) ;
#6483 = CARTESIAN_POINT ( 'NONE',  ( 41.64333658814960870, 98.77977050742731535, 30.00020018409699318 ) ) ;
#6484 = AXIS2_PLACEMENT_3D ( 'NONE', #21065, #6056, #12893 ) ;
#6485 = ORIENTED_EDGE ( 'NONE', *, *, #3835, .T. ) ;
#6486 = CARTESIAN_POINT ( 'NONE',  ( -141.4692556286852891, -167.9130981290892919, 46.40781461928724383 ) ) ;
#6487 = VERTEX_POINT ( 'NONE', #10965 ) ;
#6488 = CARTESIAN_POINT ( 'NONE',  ( 41.46631938032478359, 81.38445800887257064, 38.96596240072933170 ) ) ;
#6489 = DIRECTION ( 'NONE',  ( 1.000000000000000000, 0.000000000000000000, 0.000000000000000000 ) ) ;
#6490 = CARTESIAN_POINT ( 'NONE',  ( 43.01140435219951286, 143.9604996726487514, 28.95336869806222779 ) ) ;
#6492 = CARTESIAN_POINT ( 'NONE',  ( 19.41497643977705323, 135.2012136132025546, 3.803670830490076149 ) ) ;
#6491 = CARTESIAN_POINT ( 'NONE',  ( 38.58424406990784661, 99.26518717409396686, 35.64915139335016647 ) ) ;
#6493 = EDGE_CURVE ( 'NONE', #9727, #9693, #2880, .T. ) ;
#6494 = LINE ( 'NONE', #21381, #19691 ) ;
#6495 = CARTESIAN_POINT ( 'NONE',  ( -142.0420953463935803, -165.5084106276439968, 46.59394152635518793 ) ) ;
#6496 = CARTESIAN_POINT ( 'NONE',  ( -159.0959885057557983, -187.5938272943107279, 55.19815736654470584 ) ) ;
#6498 = CARTESIAN_POINT ( 'NONE',  ( -158.9748091281504401, -116.9891397928655010, 36.65701158161628115 ) ) ;
#6497 = CARTESIAN_POINT ( 'NONE',  ( 2.004595370269653287, 635.3380690778678854, -23.16745088979876499 ) ) ;
#6499 = FACE_OUTER_BOUND ( 'NONE', #5374, .T. ) ;
#6500 = CARTESIAN_POINT ( 'NONE',  ( 38.01140435219952707, 147.8604996726487570, 35.83527830041809636 ) ) ;
#6501 = CARTESIAN_POINT ( 'NONE',  ( 39.92123440845005433, 79.16049967264873999, 38.46393386101375711 ) ) ;
#6502 = CARTESIAN_POINT ( 'NONE',  ( 47.43856463449118621, 61.61518717409400381, 34.21067981925357060 ) ) ;
#6503 = CARTESIAN_POINT ( 'NONE',  ( -159.5594255724347761, -184.8630981290893089, 43.77915905869157598 ) ) ;
#6504 = CARTESIAN_POINT ( 'NONE',  ( 13.78455932396994577, 137.7305411390292420, 2.696406107442721467 ) ) ;
#6505 = VECTOR ( 'NONE', #11206, 1000.000000000000000 ) ;
#6506 = CARTESIAN_POINT ( 'NONE',  ( 46.59305225739526435, 145.9151871740940294, 31.60846029578754468 ) ) ;
#6507 = CARTESIAN_POINT ( 'NONE',  ( -159.0959885057557983, -157.5938272943107279, 55.19815736654470584 ) ) ;
#6508 = CARTESIAN_POINT ( 'NONE',  ( -160.8964159109769696, -182.1584106276440309, 49.65701158161630957 ) ) ;
#6509 = VERTEX_POINT ( 'NONE', #13939 ) ;
#6510 = CARTESIAN_POINT ( 'NONE',  ( 39.92123440845005433, 78.23445800887257917, 38.46393386101375711 ) ) ;
#6511 = CARTESIAN_POINT ( 'NONE',  ( -154.3824083646099439, -173.7584106276440536, 40.69124936498395328 ) ) ;
#6512 = CARTESIAN_POINT ( 'NONE',  ( 8.710246811478747020, 120.8788544656517274, 15.12029029225770316 ) ) ;
#6513 = CARTESIAN_POINT ( 'NONE',  ( 39.42975644700377558, 129.4151871740940010, 36.81289934271958941 ) ) ;
#6514 = ADVANCED_FACE ( 'NONE', ( #17353 ), #20891, .F. ) ;
#6515 = CARTESIAN_POINT ( 'NONE',  ( 40.51949181395973199, 85.84442682937354618, -12.58519764931165241 ) ) ;
#6516 = ORIENTED_EDGE ( 'NONE', *, *, #18362, .F. ) ;
#6517 = ORIENTED_EDGE ( 'NONE', *, *, #14589, .F. ) ;
#6518 = CARTESIAN_POINT ( 'NONE',  ( 43.01140435219951286, 137.0344580088725763, 29.21067981925356705 ) ) ;
#6519 = ORIENTED_EDGE ( 'NONE', *, *, #1610, .F. ) ;
#6520 = EDGE_CURVE ( 'NONE', #13207, #20212, #1607, .T. ) ;
#6521 = CARTESIAN_POINT ( 'NONE',  ( 46.10157429594899270, 106.7344580088725507, 29.95742577749337343 ) ) ;
#6522 = CARTESIAN_POINT ( 'NONE',  ( -166.4803626276155626, -116.9891397928655010, 49.65701158161629536 ) ) ;
#6523 = CARTESIAN_POINT ( 'NONE',  ( 47.43856463449117200, 68.02977050742731535, 32.77220824515698183 ) ) ;
#6525 = CARTESIAN_POINT ( 'NONE',  ( 59.83664469576316236, 97.27638873328486113, 6.703993115985443119 ) ) ;
#6524 = CARTESIAN_POINT ( 'NONE',  ( 47.43856463449118621, 121.6151871740940038, 34.21067981925357060 ) ) ;
#6526 = EDGE_CURVE ( 'NONE', #6147, #21749, #19338, .T. ) ;
#6527 = CARTESIAN_POINT ( 'NONE',  ( 47.05648932407426344, 82.91049967264873999, 37.14960608071593384 ) ) ;
#6528 = CARTESIAN_POINT ( 'NONE',  ( 12.61881386508366809, 104.1535352963828984, 15.55354899318430739 ) ) ;
#6529 = VECTOR ( 'NONE', #12728, 1000.000000000000114 ) ;
#6530 = CARTESIAN_POINT ( 'NONE',  ( 42.21948215057684450, 145.3836182503284817, 39.21067981925355639 ) ) ;
#6531 = DIRECTION ( 'NONE',  ( -0.000000000000000000, 0.000000000000000000, -1.000000000000000000 ) ) ;
#6532 = CARTESIAN_POINT ( 'NONE',  ( 44.37947211624943833, 92.21518717409401233, 30.00020018409699318 ) ) ;
#6533 = LINE ( 'NONE', #13253, #1676 ) ;
#6534 = CARTESIAN_POINT ( 'NONE',  ( -151.4692556286852891, -196.9891397928655010, 59.65701158161632378 ) ) ;
#6535 = ORIENTED_EDGE ( 'NONE', *, *, #2025, .F. ) ;
#6536 = CARTESIAN_POINT ( 'NONE',  ( 43.01140435219951286, 70.12977050742732388, 38.86567161673127657 ) ) ;
#6537 = CARTESIAN_POINT ( 'NONE',  ( -143.8425227516148084, -156.6938272943107222, 55.19815736654470584 ) ) ;
#6538 = CARTESIAN_POINT ( 'NONE',  ( 9.468627745026951814, 113.0646104733145592, 1.862908727141013854 ) ) ;
#6539 = CARTESIAN_POINT ( 'NONE',  ( -148.5561028927606344, -189.0584106276440650, 40.69124936498395328 ) ) ;
#6540 = VERTEX_POINT ( 'NONE', #12509 ) ;
#6541 = CARTESIAN_POINT ( 'NONE',  ( 44.37947211624943833, 152.2151871740940123, 30.00020018409699318 ) ) ;
#6542 = CARTESIAN_POINT ( 'NONE',  ( 45.74753988029934249, 119.3297705074273267, 30.44471234641812174 ) ) ;
#6543 = CARTESIAN_POINT ( 'NONE',  ( 71.14040157825178312, 139.4183699182763974, -9.089337262093875935 ) ) ;
#6544 = EDGE_LOOP ( 'NONE', ( #10737, #15683 ) ) ;
#6545 = AXIS2_PLACEMENT_3D ( 'NONE', #267, #5018, #8439 ) ;
#6546 = EDGE_CURVE ( 'NONE', #19216, #10835, #2369, .T. ) ;
#6547 = CARTESIAN_POINT ( 'NONE',  ( 66.16974147772015158, 135.9983230778657344, -9.010293137571032673 ) ) ;
#6548 = EDGE_LOOP ( 'NONE', ( #17582, #11767, #6991, #9856 ) ) ;
#6549 = CARTESIAN_POINT ( 'NONE',  ( 39.42975644700377558, 120.6797705074273210, 36.81289934271958941 ) ) ;
#6550 = DIRECTION ( 'NONE',  ( -1.000000000000000000, 0.000000000000000000, -0.000000000000000000 ) ) ;
#6551 = CARTESIAN_POINT ( 'NONE',  ( 47.43856463449118621, 154.6151871740940180, 34.21067981925357060 ) ) ;
#6552 = CARTESIAN_POINT ( 'NONE',  ( 32.31036143884366396, 152.4250368413922274, -10.51794503956956817 ) ) ;
#6553 = CARTESIAN_POINT ( 'NONE',  ( 83.67254549292280785, -61.68114226949890622, -16.21320343559643717 ) ) ;
#6554 = SURFACE_STYLE_FILL_AREA ( #18456 ) ;
#6555 = DIRECTION ( 'NONE',  ( 0.5010362705417044094, 0.000000000000000000, -0.8654262854811263228 ) ) ;
#6556 = VECTOR ( 'NONE', #5445, 1000.000000000000114 ) ;
#6557 = CARTESIAN_POINT ( 'NONE',  ( -157.6495955161842062, -182.0391397928654840, 58.16351966513671812 ) ) ;
#6558 = EDGE_CURVE ( 'NONE', #11465, #11702, #15704, .T. ) ;
#6559 = DIRECTION ( 'NONE',  ( 0.000000000000000000, 0.000000000000000000, -1.000000000000000000 ) ) ;
#6560 = CARTESIAN_POINT ( 'NONE',  ( -47.86331837773882825, 0.000000000000000000, -35.00000000000000000 ) ) ;
#6561 = CARTESIAN_POINT ( 'NONE',  ( -159.0959885057557983, -194.1938272943107222, 44.11586579668791330 ) ) ;
#6562 = PRODUCT ( 'Material Hold-Down Screw Clamp', 'Material Hold-Down Screw Clamp', '', ( #14484 ) ) ;
#6563 = ITEM_DEFINED_TRANSFORMATION ( 'NONE', 'NONE', #16531,  #12657 ) ;
#6564 = CARTESIAN_POINT ( 'NONE',  ( 43.01140435219951286, 126.5344580088725763, 39.46799094044489209 ) ) ;
#6565 = VECTOR ( 'NONE', #4530, 1000.000000000000114 ) ;
#6566 = CARTESIAN_POINT ( 'NONE',  ( 43.01140435219951286, 97.12977050742732388, 38.86567161673127657 ) ) ;
#6567 = CARTESIAN_POINT ( 'NONE',  ( 20.79828168028384994, 137.4105449198869735, 15.91385929137521771 ) ) ;
#6568 = CARTESIAN_POINT ( 'NONE',  ( -160.8964159109769696, -187.8938272943107393, 49.65701158161630957 ) ) ;
#6569 = CARTESIAN_POINT ( 'NONE',  ( 45.74753988029934249, 91.16518717409398675, 37.97664729208901235 ) ) ;
#6570 = CARTESIAN_POINT ( 'NONE',  ( 38.96631938032478359, 84.41049967264873999, 31.27175355779120025 ) ) ;
#6571 = ORIENTED_EDGE ( 'NONE', *, *, #2773, .F. ) ;
#6572 = EDGE_CURVE ( 'NONE', #6015, #14746, #19235, .T. ) ;
#6573 = CARTESIAN_POINT ( 'NONE',  ( 156.1725454929228079, -61.68114226949890622, 19.99999999999998934 ) ) ;
#6574 = CARTESIAN_POINT ( 'NONE',  ( 9.203281625063985061, 114.5318647093721864, 15.91056058043385413 ) ) ;
#6575 =( BOUNDED_CURVE ( )  B_SPLINE_CURVE ( 2, ( #19958, #4619, #10144, #6501, #20074, #11340, #9925, #19838, #16739, #14865, #11671, #1651, #18293 ),
 .UNSPECIFIED., .F., .F. ) 
 B_SPLINE_CURVE_WITH_KNOTS ( ( 3, 2, 2, 2, 2, 2, 3 ),
 ( 0.7867647058823529216, 0.7882352941176470340, 0.7911764705882352589, 0.7941176470588234837, 0.7970588235294118196, 0.8000000000000000444, 0.8014705882352941568 ),
 .UNSPECIFIED. ) 
 CURVE ( )  GEOMETRIC_REPRESENTATION_ITEM ( )  RATIONAL_B_SPLINE_CURVE ( ( 0.9755282581475768211, 0.9755282581475768211, 1.000000000000000000, 0.9510565162951535312, 1.000000000000000000, 0.9510565162951535312, 1.000000000000000000, 0.9510565162951535312, 1.000000000000000000, 0.9510565162951535312, 1.000000000000000000, 0.9755282581475768211, 0.9755282581475768211 ) ) 
 REPRESENTATION_ITEM ( '' )  );
#6576 = CARTESIAN_POINT ( 'NONE',  ( 55.97020510223934764, 144.8627979930266463, -1.553355716038981038 ) ) ;
#6577 = CARTESIAN_POINT ( 'NONE',  ( 39.42975644700377558, 69.07977050742732672, 31.60846029578754468 ) ) ;
#6578 = ORIENTED_EDGE ( 'NONE', *, *, #13365, .F. ) ;
#6579 = AXIS2_PLACEMENT_3D ( 'NONE', #4194, #16191, #21066 ) ;
#6580 = CARTESIAN_POINT ( 'NONE',  ( 47.43856463449117200, 143.0297705074273154, 32.77220824515698183 ) ) ;
#6581 = CARTESIAN_POINT ( 'NONE',  ( 47.43856463449117200, 98.02977050742731535, 32.77220824515698183 ) ) ;
#6582 = MECHANICAL_DESIGN_GEOMETRIC_PRESENTATION_REPRESENTATION (  '', ( #2350 ), #18555 ) ;
#6583 = CARTESIAN_POINT ( 'NONE',  ( -153.0531000319306543, -192.8899795514095672, 59.65701158161632378 ) ) ;
#6584 = CARTESIAN_POINT ( 'NONE',  ( 38.01140435219951996, 108.8604996726487144, 35.83527830041810347 ) ) ;
#6585 = CARTESIAN_POINT ( 'NONE',  ( 39.42975644700377558, 71.81518717409400665, 31.60846029578754468 ) ) ;
#6586 = CARTESIAN_POINT ( 'NONE',  ( -155.3247660971250923, -155.7098880568450454, 40.99743995317548695 ) ) ;
#6587 = CARTESIAN_POINT ( 'NONE',  ( -151.4692556286852891, -161.6438272943107393, 39.74470866294723947 ) ) ;
#6588 = CARTESIAN_POINT ( 'NONE',  ( -141.4692556286852891, -165.8391397928654669, 46.40781461928724383 ) ) ;
#6589 = CARTESIAN_POINT ( 'NONE',  ( -161.4692556286853176, -181.5630981290892976, 49.65701158161630957 ) ) ;
#6590 = DIRECTION ( 'NONE',  ( 0.000000000000000000, 0.000000000000000000, 1.000000000000000000 ) ) ;
#6591 = CARTESIAN_POINT ( 'NONE',  ( -159.5594255724347761, -191.7891397928654555, 43.77915905869157598 ) ) ;
#6592 = CARTESIAN_POINT ( 'NONE',  ( 38.96631938032478359, 153.0844580088725877, 37.14960608071593384 ) ) ;
#6593 = CARTESIAN_POINT ( 'NONE',  ( 45.74753988029933538, 125.3297705074273125, 30.44471234641811819 ) ) ;
#6594 = CARTESIAN_POINT ( 'NONE',  ( 14.94030450088465400, 100.1727563578744196, 14.40630071170483362 ) ) ;
#6595 = CARTESIAN_POINT ( 'NONE',  ( 46.59305225739526435, 118.9151871740940010, 31.60846029578754468 ) ) ;
#6596 = EDGE_CURVE ( 'NONE', #16002, #20743, #4558, .T. ) ;
#6597 = CARTESIAN_POINT ( 'NONE',  ( -161.4692556286852891, -167.3391397928654101, 52.90620854394536821 ) ) ;
#6598 = CARTESIAN_POINT ( 'NONE',  ( 47.05648932407426344, 64.91049967264873999, 37.14960608071593384 ) ) ;
#6599 = CARTESIAN_POINT ( 'NONE',  ( 25.37887452999470028, 90.65668055682171200, 1.938985092122112563 ) ) ;
#6600 = CARTESIAN_POINT ( 'NONE',  ( 22.56676867748217674, 139.3294883087844198, 3.013676707730225779 ) ) ;
#6601 = CARTESIAN_POINT ( 'NONE',  ( 72.34521997529867576, 314.8592298662555322, 272.0939500981630204 ) ) ;
#6602 = CARTESIAN_POINT ( 'NONE',  ( 46.59305225739526435, 95.17977050742732104, 31.60846029578754468 ) ) ;
#6603 = ORIENTED_EDGE ( 'NONE', *, *, #13085, .T. ) ;
#6604 = VECTOR ( 'NONE', #12703, 1000.000000000000000 ) ;
#6605 = CARTESIAN_POINT ( 'NONE',  ( 44.55648932407425633, 145.8844580088725991, 29.45539723777780239 ) ) ;
#6606 = ORIENTED_EDGE ( 'NONE', *, *, #12774, .T. ) ;
#6607 = CARTESIAN_POINT ( 'NONE',  ( 47.05648932407426344, 81.98445800887257917, 37.14960608071593384 ) ) ;
#6608 = CARTESIAN_POINT ( 'NONE',  ( 159.0505745212445561, 203.5296818892961994, 14.00000000000001776 ) ) ;
#6609 = EDGE_CURVE ( 'NONE', #12140, #1305, #21556, .T. ) ;
#6610 = AXIS2_PLACEMENT_3D ( 'NONE', #14704, #14590, #21667 ) ;
#6611 = PRODUCT_DEFINITION_SHAPE ( 'NONE', 'NONE',  #21822 ) ;
#6612 = CARTESIAN_POINT ( 'NONE',  ( 48.01140435219951996, 140.2104996726487514, 34.21067981925357060 ) ) ;
#6614 = CARTESIAN_POINT ( 'NONE',  ( 45.08035905667198762, 147.9511986603014861, 4.994099723559113357 ) ) ;
#6613 = CARTESIAN_POINT ( 'NONE',  ( 46.59305225739526435, 97.91518717409400097, 31.60846029578754468 ) ) ;
#6615 = CARTESIAN_POINT ( 'NONE',  ( -151.4692556286852891, -169.4084106276440593, 59.56931450028537967 ) ) ;
#6616 = CARTESIAN_POINT ( 'NONE',  ( -142.0420953463935803, -186.2438272943107336, 46.59394152635518083 ) ) ;
#6618 = CARTESIAN_POINT ( 'NONE',  ( 44.55648932407425633, 70.88445800887258486, 29.45539723777780239 ) ) ;
#6617 = CARTESIAN_POINT ( 'NONE',  ( 173.3794444120442506, -126.9891397928655010, 30.00000000000000000 ) ) ;
#6619 = DIRECTION ( 'NONE',  ( 1.000000000000000000, 0.000000000000000000, 0.000000000000000000 ) ) ;
#6620 = CARTESIAN_POINT ( 'NONE',  ( 43.01140435219951996, 148.4604996726487798, 39.21067981925356349 ) ) ;
#6621 = CARTESIAN_POINT ( 'NONE',  ( 43.01140435219951286, 114.5344580088725621, 39.21067981925356349 ) ) ;
#6622 = CARTESIAN_POINT ( 'NONE',  ( 41.64333658814960870, 158.7797705074273438, 30.00020018409699318 ) ) ;
#6623 = CYLINDRICAL_SURFACE ( 'NONE', #20008, 4.999999999999997335 ) ;
#6624 = CARTESIAN_POINT ( 'NONE',  ( 57.78275410301085913, 89.02518083909171764, -0.1607367497116551913 ) ) ;
#6625 = CARTESIAN_POINT ( 'NONE',  ( 43.01140435219951286, 149.3651871740939612, 29.55568802177586107 ) ) ;
#6626 = VECTOR ( 'NONE', #13316, 1000.000000000000000 ) ;
#6627 = CARTESIAN_POINT ( 'NONE',  ( -157.2955611005346270, -163.4438272943107506, 57.67623309621198047 ) ) ;
#6628 = CARTESIAN_POINT ( 'NONE',  ( -145.6429501568359797, -172.1084106276440195, 57.67623309621197336 ) ) ;
#6629 = VECTOR ( 'NONE', #18124, 1000.000000000000000 ) ;
#6630 = ORIENTED_EDGE ( 'NONE', *, *, #14584, .F. ) ;
#6631 = CARTESIAN_POINT ( 'NONE',  ( 47.43856463449118621, 64.61518717409398960, 34.21067981925357060 ) ) ;
#6632 = CARTESIAN_POINT ( 'NONE',  ( -159.0959885057557983, -163.8584106276440480, 55.19815736654470584 ) ) ;
#6633 = CARTESIAN_POINT ( 'NONE',  ( 42.84661501159713026, 148.1872198635363134, -4.086158671962061284 ) ) ;
#6634 = AXIS2_PLACEMENT_3D ( 'NONE', #4237, #21003, #8892 ) ;
#6635 = STYLED_ITEM ( 'NONE', ( #992 ), #7211 ) ;
#6636 = DIRECTION ( 'NONE',  ( 0.000000000000000000, 0.000000000000000000, 1.000000000000000000 ) ) ;
#6637 = CARTESIAN_POINT ( 'NONE',  ( 45.74753988029933538, 122.0651871740940209, 30.44471234641811819 ) ) ;
#6638 = EDGE_CURVE ( 'NONE', #20247, #7422, #11313, .T. ) ;
#6639 = CARTESIAN_POINT ( 'NONE',  ( 12.20328755962376199, 134.6477104347696923, -3.418325544530929516 ) ) ;
#6640 = ORIENTED_EDGE ( 'NONE', *, *, #15281, .F. ) ;
#6641 = ORIENTED_EDGE ( 'NONE', *, *, #6437, .T. ) ;
#6642 = CARTESIAN_POINT ( 'NONE',  ( -148.3790856849358306, -193.5891397928654669, 59.16757674456786020 ) ) ;
#6643 = ORIENTED_EDGE ( 'NONE', *, *, #13573, .F. ) ;
#6644 = CARTESIAN_POINT ( 'NONE',  ( 38.01140435219951996, 110.6344580088725849, 32.58608133808903773 ) ) ;
#6645 = CARTESIAN_POINT ( 'NONE',  ( 47.05648932407426344, 115.9104996726487400, 37.14960608071593384 ) ) ;
#6646 = CARTESIAN_POINT ( 'NONE',  ( 45.74753988029933538, 67.42977050742730682, 37.97664729208901946 ) ) ;
#6648 = CARTESIAN_POINT ( 'NONE',  ( 50.21395344324809429, 147.1711500555979626, 4.203964687196366512 ) ) ;
#6647 = CARTESIAN_POINT ( 'NONE',  ( 38.58424406990786082, 126.1151871740940038, 34.21067981925357060 ) ) ;
#6649 = CARTESIAN_POINT ( 'NONE',  ( 47.05648932407426344, 77.51049967264873430, 31.27175355779120025 ) ) ;
#6650 = AXIS2_PLACEMENT_3D ( 'NONE', #10707, #16681, #8215 ) ;
#6651 = FACE_OUTER_BOUND ( 'NONE', #8147, .T. ) ;
#6652 = CARTESIAN_POINT ( 'NONE',  ( 41.46631938032478359, 144.1104996726487570, 29.45539723777780239 ) ) ;
#6653 = CARTESIAN_POINT ( 'NONE',  ( 43.01140435219951286, 137.9604996726487514, 29.21067981925356705 ) ) ;
#6654 = CARTESIAN_POINT ( 'NONE',  ( 40.27526882409969033, 90.56518717409400665, 37.97664729208901946 ) ) ;
#6655 = PRODUCT_DEFINITION_CONTEXT ( 'detailed design', #4077, 'design' ) ;
#6656 = CARTESIAN_POINT ( 'NONE',  ( 39.24377615895817684, 144.6226614538730928, 30.90720150815158718 ) ) ;
#6657 = CARTESIAN_POINT ( 'NONE',  ( 156.7804311855217065, 208.8003142469820830, -29.99999999999997868 ) ) ;
#6658 = ORIENTED_EDGE ( 'NONE', *, *, #19850, .F. ) ;
#6659 = CARTESIAN_POINT ( 'NONE',  ( 40.27526882409969033, 69.82977050742729830, 37.97664729208901946 ) ) ;
#6660 = CARTESIAN_POINT ( 'NONE',  ( -151.4692556286852891, -184.4084106276440593, 59.56931450028537967 ) ) ;
#6661 = EDGE_CURVE ( 'NONE', #13376, #7553, #16350, .T. ) ;
#6662 = CARTESIAN_POINT ( 'NONE',  ( 63.41425016244589585, 92.41789933959738335, 6.624947895572852019 ) ) ;
#6663 = CARTESIAN_POINT ( 'NONE',  ( -160.8964159109769696, -179.3084106276440082, 46.59394152635518793 ) ) ;
#6664 = EDGE_LOOP ( 'NONE', ( #7979, #11135, #19992, #14094 ) ) ;
#6665 = CARTESIAN_POINT ( 'NONE',  ( 38.58424406990784661, 156.2651871740939953, 35.64915139335016647 ) ) ;
#6666 = CARTESIAN_POINT ( 'NONE',  ( -143.3790856849358306, -159.6891397928654897, 43.77915905869157598 ) ) ;
#6667 = CARTESIAN_POINT ( 'NONE',  ( 44.37947211624943833, 112.2797705074273296, 38.42115945441014446 ) ) ;
#6668 = CARTESIAN_POINT ( 'NONE',  ( 64.59149290518072917, 93.33317027722591774, -7.422718449586769296 ) ) ;
#6669 = ORIENTED_EDGE ( 'NONE', *, *, #1261, .T. ) ;
#6670 = PRESENTATION_STYLE_ASSIGNMENT (( #6879 ) ) ;
#6671 = ORIENTED_EDGE ( 'NONE', *, *, #9508, .T. ) ;
#6672 = CARTESIAN_POINT ( 'NONE',  ( 43.01140435219951286, 119.6297705074272955, 29.55568802177586463 ) ) ;
#6673 = CARTESIAN_POINT ( 'NONE',  ( 42.21948215057684450, 129.4575765865523067, 39.21067981925355639 ) ) ;
#6674 = CARTESIAN_POINT ( 'NONE',  ( 47.43856463449117200, 151.4651871740939839, 35.64915139335016647 ) ) ;
#6675 = CARTESIAN_POINT ( 'NONE',  ( 68.88151390383544026, 142.3271613368909811, -9.208263745312144977 ) ) ;
#6676 = LINE ( 'NONE', #17084, #2009 ) ;
#6677 = CARTESIAN_POINT ( 'NONE',  ( -120.0322075325610740, -136.9891397928655010, 49.65701158161630957 ) ) ;
#6678 = CARTESIAN_POINT ( 'NONE',  ( -151.4692556286852891, -196.9891397928655010, 49.65701158161630957 ) ) ;
#6679 = CARTESIAN_POINT ( 'NONE',  ( -157.6495955161842062, -179.0391397928654840, 58.16351966513671812 ) ) ;
#6680 = DIRECTION ( 'NONE',  ( 0.000000000000000000, 0.000000000000000000, 1.000000000000000000 ) ) ;
#6681 = CARTESIAN_POINT ( 'NONE',  ( 136.0032066456581390, 182.5367998656340944, 14.00000000000001776 ) ) ;
#6682 = CARTESIAN_POINT ( 'NONE',  ( 44.55648932407425633, 92.81049967264874567, 29.45539723777780239 ) ) ;
#6683 = ITEM_DEFINED_TRANSFORMATION ( 'NONE', 'NONE', #8476,  #12657 ) ;
#6684 = CIRCLE ( 'NONE', #12641, 10.00000000000000888 ) ;
#6685 = CARTESIAN_POINT ( 'NONE',  ( 38.58424406990786082, 93.37977050742732388, 34.21067981925357060 ) ) ;
#6686 = CARTESIAN_POINT ( 'NONE',  ( 28.77282558494574971, 95.47244942437217219, 14.00900696324737282 ) ) ;
#6687 = CARTESIAN_POINT ( 'NONE',  ( -159.0959885057557983, -173.1938272943107506, 44.11586579668791330 ) ) ;
#6688 = EDGE_CURVE ( 'NONE', #6320, #13485, #1258, .T. ) ;
#6689 = CARTESIAN_POINT ( 'NONE',  ( 47.43856463449118621, 88.61518717409400381, 34.21067981925357060 ) ) ;
#6690 = CARTESIAN_POINT ( 'NONE',  ( 161.4980277546683283, 196.8248625098966897, 21.73429951086134082 ) ) ;
#6691 = ORIENTED_EDGE ( 'NONE', *, *, #14114, .F. ) ;
#6692 = CARTESIAN_POINT ( 'NONE',  ( -143.3790856849358306, -189.6891397928654612, 43.77915905869157598 ) ) ;
#6693 = CARTESIAN_POINT ( 'NONE',  ( 10.91571581598819662, 131.8149664739095783, 9.482090752819161139 ) ) ;
#6694 = CARTESIAN_POINT ( 'NONE',  ( 45.74753988029934249, 139.4297705074272642, 37.97664729208901235 ) ) ;
#6695 = CARTESIAN_POINT ( 'NONE',  ( 15.97902590142590462, 112.1642626292039324, 2.851329040111875823 ) ) ;
#6696 = DIRECTION ( 'NONE',  ( 1.000000000000000000, 0.000000000000000000, 0.000000000000000000 ) ) ;
#6697 = ORIENTED_EDGE ( 'NONE', *, *, #18056, .F. ) ;
#6698 = CARTESIAN_POINT ( 'NONE',  ( 47.43856463449118621, 142.8797705074273381, 34.21067981925357060 ) ) ;
#6699 = VECTOR ( 'NONE', #7020, 1000.000000000000000 ) ;
#6700 = CARTESIAN_POINT ( 'NONE',  ( 45.74753988029933538, 95.32977050742729830, 30.44471234641811819 ) ) ;
#6701 = CARTESIAN_POINT ( 'NONE',  ( 44.55648932407425633, 151.6104996726487570, 38.96596240072933170 ) ) ;
#6702 = ADVANCED_FACE ( 'NONE', ( #7778 ), #17889, .F. ) ;
#6703 = CARTESIAN_POINT ( 'NONE',  ( 48.01140435219951996, 110.0604996726487315, 35.83527830041810347 ) ) ;
#6704 = LINE ( 'NONE', #13411, #12909 ) ;
#6705 = FACE_OUTER_BOUND ( 'NONE', #12501, .T. ) ;
#6706 = CARTESIAN_POINT ( 'NONE',  ( -159.0959885057557983, -163.5938272943107279, 55.19815736654470584 ) ) ;
#6707 = CARTESIAN_POINT ( 'NONE',  ( 163.3167426812955227, 191.7976672453297624, 20.78115173001200944 ) ) ;
#6708 = CARTESIAN_POINT ( 'NONE',  ( -159.5594255724347761, -169.8630981290893089, 43.77915905869157598 ) ) ;
#6709 = CARTESIAN_POINT ( 'NONE',  ( 47.43856463449117200, 118.7297705074272898, 35.64915139335016647 ) ) ;
#6710 =( BOUNDED_CURVE ( )  B_SPLINE_CURVE ( 2, ( #3174, #11544, #11319, #16492, #20052, #14952, #4599, #21478, #18270, #2948, #1084, #16283, #1411 ),
 .UNSPECIFIED., .F., .F. ) 
 B_SPLINE_CURVE_WITH_KNOTS ( ( 3, 2, 2, 2, 2, 2, 3 ),
 ( 0.1838235294117647189, 0.1852941176470588314, 0.1882352941176470562, 0.1911764705882352811, 0.1941176470588235337, 0.1970588235294117585, 0.1985294117647058987 ),
 .UNSPECIFIED. ) 
 CURVE ( )  GEOMETRIC_REPRESENTATION_ITEM ( )  RATIONAL_B_SPLINE_CURVE ( ( 0.9755282581475768211, 0.9755282581475770431, 1.000000000000000000, 0.9510565162951535312, 1.000000000000000000, 0.9510565162951535312, 1.000000000000000000, 0.9510565162951535312, 1.000000000000000000, 0.9510565162951535312, 1.000000000000000000, 0.9755282581475765991, 0.9755282581475768211 ) ) 
 REPRESENTATION_ITEM ( '' )  );
#6711 = CARTESIAN_POINT ( 'NONE',  ( 32.32016755483360271, 87.30015788337030358, 13.69171886368053492 ) ) ;
#6712 = CARTESIAN_POINT ( 'NONE',  ( 46.10157429594899270, 95.66049967264872578, 29.95742577749336988 ) ) ;
#6713 = CARTESIAN_POINT ( 'NONE',  ( 45.74753988029934249, 112.1651871740939868, 37.97664729208901235 ) ) ;
#6714 = CARTESIAN_POINT ( 'NONE',  ( -153.0531000319306827, -166.8160212151857138, 59.65701158161631668 ) ) ;
#6715 = COLOUR_RGB ( '', 0.66274510, 0.83137255, 0.94901961) ;
#6716 = DIRECTION ( 'NONE',  ( -1.000000000000000000, 0.000000000000000000, 0.000000000000000000 ) ) ;
#6717 = CARTESIAN_POINT ( 'NONE',  ( 8.886384673113061794, 121.3059481585812733, 3.129088064915290346 ) ) ;
#6718 = CARTESIAN_POINT ( 'NONE',  ( 64.66009251794113766, 101.8366349233107684, -0.5580327111990067701 ) ) ;
#6719 = DIRECTION ( 'NONE',  ( -1.000000000000000000, 0.000000000000000000, 0.000000000000000000 ) ) ;
#6720 = CARTESIAN_POINT ( 'NONE',  ( 47.43856463449117911, 86.02977050742731535, 32.77220824515697473 ) ) ;
#6721 = ORIENTED_EDGE ( 'NONE', *, *, #6806, .F. ) ;
#6722 = CARTESIAN_POINT ( 'NONE',  ( -141.4692556286852891, -195.9891397928654726, 49.65701158161630957 ) ) ;
#6723 = ORIENTED_EDGE ( 'NONE', *, *, #5537, .F. ) ;
#6724 = CARTESIAN_POINT ( 'NONE',  ( 39.92123440845004723, 74.33445800887255928, 29.95742577749337343 ) ) ;
#6725 = LINE ( 'NONE', #11883, #16156 ) ;
#6726 = EDGE_CURVE ( 'NONE', #21815, #16287, #9432, .T. ) ;
#6727 = CARTESIAN_POINT ( 'NONE',  ( 38.01140435219951996, 138.5604996726487457, 32.58608133808903773 ) ) ;
#6729 = CARTESIAN_POINT ( 'NONE',  ( 61.38527826276358468, 91.11739401521901982, -13.29920278214092200 ) ) ;
#6728 = CARTESIAN_POINT ( 'NONE',  ( 41.64333658814960870, 95.51518717409400949, 30.00020018409699318 ) ) ;
#6730 = CARTESIAN_POINT ( 'NONE',  ( -145.6429501568359797, -166.1084106276440480, 57.67623309621198047 ) ) ;
#6731 = CARTESIAN_POINT ( 'NONE',  ( -160.8964159109769696, -190.7438272943107336, 52.72008163687743121 ) ) ;
#6733 = CARTESIAN_POINT ( 'NONE',  ( 48.01140435219951996, 70.43445800887256780, 32.58608133808903773 ) ) ;
#6732 = CARTESIAN_POINT ( 'NONE',  ( -161.4692556286853176, -166.5630981290893260, 49.65701158161630957 ) ) ;
#6734 = CARTESIAN_POINT ( 'NONE',  ( -151.4692556286852891, -188.3130981290893260, 39.65701158161629536 ) ) ;
#6735 = DIRECTION ( 'NONE',  ( 0.9387810623359076345, 0.3426822732243071656, 0.03548206049944094970 ) ) ;
#6736 = CARTESIAN_POINT ( 'NONE',  ( 47.05648932407426344, 79.91049967264873999, 37.14960608071593384 ) ) ;
#6737 = CARTESIAN_POINT ( 'NONE',  ( 39.42975644700377558, 147.0797705074273267, 31.60846029578754468 ) ) ;
#6738 = CARTESIAN_POINT ( 'NONE',  ( -55.11860757350579831, 784.8075632535900468, -19.99999999999997868 ) ) ;
#6739 = CARTESIAN_POINT ( 'NONE',  ( 76.04618105687035268, 128.8835079444423286, -1.708432735116285350 ) ) ;
#6740 = CARTESIAN_POINT ( 'NONE',  ( 45.74753988029934249, 149.0651871740940067, 30.44471234641812174 ) ) ;
#6741 = CARTESIAN_POINT ( 'NONE',  ( -157.2955611005346270, -160.4438272943106654, 57.67623309621198047 ) ) ;
#6742 = CARTESIAN_POINT ( 'NONE',  ( -160.8964159109769696, -176.1584106276440309, 49.65701158161630957 ) ) ;
#6743 = ORIENTED_EDGE ( 'NONE', *, *, #7316, .F. ) ;
#6744 = CARTESIAN_POINT ( 'NONE',  ( 40.27526882409969744, 62.66518717409400097, 30.44471234641812174 ) ) ;
#6745 = CARTESIAN_POINT ( 'NONE',  ( -143.8425227516148084, -156.9584106276440423, 55.19815736654470584 ) ) ;
#6746 = CARTESIAN_POINT ( 'NONE',  ( 61.02373258766779429, 98.10483126312279012, -1.347972122102980119 ) ) ;
#6747 = CARTESIAN_POINT ( 'NONE',  ( 38.96631938032478359, 135.0844580088725877, 37.14960608071593384 ) ) ;
#6748 = CARTESIAN_POINT ( 'NONE',  ( 41.64333658814960870, 120.7151871740939981, 38.42115945441014446 ) ) ;
#6749 = ORIENTED_EDGE ( 'NONE', *, *, #88, .F. ) ;
#6750 = ORIENTED_EDGE ( 'NONE', *, *, #2230, .F. ) ;
#6751 = CARTESIAN_POINT ( 'NONE',  ( 43.01140435219951286, 135.5344580088725763, 39.21067981925356349 ) ) ;
#6752 = ORIENTED_EDGE ( 'NONE', *, *, #5669, .T. ) ;
#6753 = CARTESIAN_POINT ( 'NONE',  ( 38.96631938032478359, 111.0844580088725735, 37.14960608071593384 ) ) ;
#6754 = CARTESIAN_POINT ( 'NONE',  ( -130.4480969619998234, -126.9891397928655010, 67.64809332337415526 ) ) ;
#6755 = CARTESIAN_POINT ( 'NONE',  ( 43.01140435219951286, 64.12977050742730967, 38.86567161673127657 ) ) ;
#6757 = CARTESIAN_POINT ( 'NONE',  ( 16.56453993303484395, 129.6948329502664308, 9.561135973024818213 ) ) ;
#6756 = CARTESIAN_POINT ( 'NONE',  ( 46.59305225739526435, 130.3151871740940067, 36.81289934271958941 ) ) ;
#6758 = CARTESIAN_POINT ( 'NONE',  ( 48.01140435219951996, 86.06049967264874567, 35.83527830041810347 ) ) ;
#6759 = CARTESIAN_POINT ( 'NONE',  ( 12.43312601512511151, 135.2277911470865490, 16.60371454366222466 ) ) ;
#6760 = CARTESIAN_POINT ( 'NONE',  ( 43.01140435219951996, 70.71049967264875136, 39.21067981925356349 ) ) ;
#6761 = CARTESIAN_POINT ( 'NONE',  ( 54.85617982533818804, 239.2521282348021714, -19.99999999999996092 ) ) ;
#6762 = CARTESIAN_POINT ( 'NONE',  ( 38.58424406990786082, 78.11518717409400381, 34.21067981925357060 ) ) ;
#6763 = CARTESIAN_POINT ( 'NONE',  ( 145.5008360144876747, 198.5836349573982886, 34.00000000000001421 ) ) ;
#6764 = DIRECTION ( 'NONE',  ( -0.000000000000000000, -0.000000000000000000, -1.000000000000000000 ) ) ;
#6765 = ORIENTED_EDGE ( 'NONE', *, *, #6572, .F. ) ;
#6766 = CARTESIAN_POINT ( 'NONE',  ( 45.74753988029933538, 67.42977050742730682, 37.97664729208901946 ) ) ;
#6767 = CARTESIAN_POINT ( 'NONE',  ( -143.8425227516148084, -183.3584106276440480, 44.11586579668791330 ) ) ;
#6768 = CARTESIAN_POINT ( 'NONE',  ( 55.94180145820917716, 151.6039095241057453, 11.26783467880839140 ) ) ;
#6769 = CARTESIAN_POINT ( 'NONE',  ( -160.8964159109769696, -179.0084106276440252, 52.72008163687743121 ) ) ;
#6770 = EDGE_LOOP ( 'NONE', ( #13574, #16129, #16912, #9618 ) ) ;
#6771 = VECTOR ( 'NONE', #18889, 1000.000000000000000 ) ;
#6772 =( REPRESENTATION_RELATIONSHIP ('NONE','NONE', #6933, #8609 ) REPRESENTATION_RELATIONSHIP_WITH_TRANSFORMATION ( #6563 )SHAPE_REPRESENTATION_RELATIONSHIP( ) );
#6773 = CARTESIAN_POINT ( 'NONE',  ( 47.43856463449117200, 157.4651871740940123, 35.64915139335016647 ) ) ;
#6774 = AXIS2_PLACEMENT_3D ( 'NONE', #15663, #15358, #10290 ) ;
#6775 = CARTESIAN_POINT ( 'NONE',  ( 43.01140435219951996, 119.9070776186055838, -19.99999999999998579 ) ) ;
#6776 = CARTESIAN_POINT ( 'NONE',  ( 44.37947211624943833, 110.4797705074273324, 30.00020018409699318 ) ) ;
#6777 = CARTESIAN_POINT ( 'NONE',  ( 43.80332655382220253, 153.6113394311928744, 39.21067981925355639 ) ) ;
#6778 = EDGE_LOOP ( 'NONE', ( #3323, #4299, #3378, #21486 ) ) ;
#6779 = CARTESIAN_POINT ( 'NONE',  ( 46.66836841558743032, 147.8683539324387368, -2.938892455568735240 ) ) ;
#6780 = EDGE_LOOP ( 'NONE', ( #20219, #9123 ) ) ;
#6781 = CARTESIAN_POINT ( 'NONE',  ( 47.43856463449118621, 115.8797705074273097, 34.21067981925357060 ) ) ;
#6782 = CARTESIAN_POINT ( 'NONE',  ( 93.25569916848381524, 126.0916958004080755, 272.0939500981630204 ) ) ;
#6783 = CARTESIAN_POINT ( 'NONE',  ( 41.64333658814960870, 155.5151871740940237, 30.00020018409699318 ) ) ;
#6784 = CARTESIAN_POINT ( 'NONE',  ( 21.64910689156460322, 146.5545592879464607, 4.081561387450916456 ) ) ;
#6785 = AXIS2_PLACEMENT_3D ( 'NONE', #5500, #657, #3755 ) ;
#6786 = AXIS2_PLACEMENT_3D ( 'NONE', #7602, #21047, #2949 ) ;
#6787 = DIRECTION ( 'NONE',  ( -0.9999746145782334450, 0.007125320983193088667, 0.000000000000000000 ) ) ;
#6788 = CARTESIAN_POINT ( 'NONE',  ( -262.4284940691236443, 713.9312056531381359, 0.000000000000000000 ) ) ;
#6789 = EDGE_CURVE ( 'NONE', #20418, #4860, #12398, .T. ) ;
#6790 = CARTESIAN_POINT ( 'NONE',  ( -148.3790856849358306, -180.3891397928654783, 40.14644641866477315 ) ) ;
#6791 = CARTESIAN_POINT ( 'NONE',  ( -161.4692556286852891, -194.3391397928654669, 52.90620854394536821 ) ) ;
#6792 = CARTESIAN_POINT ( 'NONE',  ( 48.01140435219951996, 77.21049967264873715, 34.21067981925357060 ) ) ;
#6793 = VECTOR ( 'NONE', #2687, 1000.000000000000227 ) ;
#6794 = CARTESIAN_POINT ( 'NONE',  ( 38.58424406990784661, 90.22977050742731819, 32.77220824515698183 ) ) ;
#6795 = CARTESIAN_POINT ( 'NONE',  ( 57.39747520560054284, 144.1616143014069280, -9.486357586414486676 ) ) ;
#6796 = CARTESIAN_POINT ( 'NONE',  ( -159.0959885057557983, -172.5938272943107279, 55.19815736654470584 ) ) ;
#6797 = CARTESIAN_POINT ( 'NONE',  ( 38.58424406990785371, 86.96518717409398391, 32.77220824515697473 ) ) ;
#6798 = CARTESIAN_POINT ( 'NONE',  ( -141.4692556286852891, -195.9891397928654726, 49.65701158161630957 ) ) ;
#6799 = ORIENTED_EDGE ( 'NONE', *, *, #4788, .F. ) ;
#6800 = DIRECTION ( 'NONE',  ( -1.000000000000000000, 0.000000000000000000, -4.622506457652816058E-16 ) ) ;
#6801 = CARTESIAN_POINT ( 'NONE',  ( 70.62757080055673953, 99.67629488849819097, 13.29148015538516425 ) ) ;
#6802 = CARTESIAN_POINT ( 'NONE',  ( 58.57598713290192904, 143.3259681031794059, -1.434385245616870197 ) ) ;
#6803 = CARTESIAN_POINT ( 'NONE',  ( 39.92123440845005433, 119.3344580088725735, 29.95742577749336988 ) ) ;
#6804 = VERTEX_POINT ( 'NONE', #3134 ) ;
#6805 = CARTESIAN_POINT ( 'NONE',  ( 41.64333658814960870, 149.7797705074273154, 30.00020018409699318 ) ) ;
#6806 = EDGE_CURVE ( 'NONE', #9507, #119, #14807, .T. ) ;
#6807 = CARTESIAN_POINT ( 'NONE',  ( 43.01140435219951286, 98.62977050742730967, 29.55568802177586463 ) ) ;
#6809 = EDGE_CURVE ( 'NONE', #2742, #11679, #14504, .T. ) ;
#6808 = CARTESIAN_POINT ( 'NONE',  ( 38.96631938032478359, 141.4104996726487400, 31.27175355779120025 ) ) ;
#6810 = CARTESIAN_POINT ( 'NONE',  ( -151.4692556286852891, -196.9891397928655010, 49.65701158161630957 ) ) ;
#6811 = PLANE ( 'NONE',  #18735 ) ;
#6812 = EDGE_CURVE ( 'NONE', #21236, #2680, #3254, .T. ) ;
#6813 = CARTESIAN_POINT ( 'NONE',  ( -141.4692556286852891, -174.2130981290893033, 52.90620854394536821 ) ) ;
#6814 = CARTESIAN_POINT ( 'NONE',  ( -133.8097529055291943, 761.2091818577913500, -6.999999999999982236 ) ) ;
#6815 = CARTESIAN_POINT ( 'NONE',  ( -157.6495955161842062, -170.0130981290892862, 41.15050349809590102 ) ) ;
#6816 = CARTESIAN_POINT ( 'NONE',  ( 48.01140435219951996, 142.4344580088725820, 32.58608133808903773 ) ) ;
#6817 = CARTESIAN_POINT ( 'NONE',  ( 38.58424406990784661, 120.5297705074273154, 35.64915139335016647 ) ) ;
#6818 = CARTESIAN_POINT ( 'NONE',  ( 15.77498628565902727, 140.7233915340666499, 22.81684008552556975 ) ) ;
#6819 = CARTESIAN_POINT ( 'NONE',  ( 38.58424406990785371, 119.9651871740939839, 32.77220824515697473 ) ) ;
#6820 = CARTESIAN_POINT ( 'NONE',  ( 46.37776046713125311, 85.92026137128108587, 1.224418530371263580 ) ) ;
#6821 = CARTESIAN_POINT ( 'NONE',  ( 41.25620118372704326, 148.0523446076144580, 3.846850258842608117 ) ) ;
#6822 = CARTESIAN_POINT ( 'NONE',  ( 109.8528842077358405, 344.7014318495014322, -19.99999999999997868 ) ) ;
#6823 = EDGE_CURVE ( 'NONE', #6422, #16834, #15124, .T. ) ;
#6824 = CARTESIAN_POINT ( 'NONE',  ( 47.43856463449118621, 82.87977050742730967, 34.21067981925357060 ) ) ;
#6825 = ORIENTED_EDGE ( 'NONE', *, *, #10439, .F. ) ;
#6826 = ADVANCED_FACE ( 'NONE', ( #6215 ), #2915, .T. ) ;
#6827 = CARTESIAN_POINT ( 'NONE',  ( 43.01140435219951996, 2.710499672648754466, 34.21067981925357060 ) ) ;
#6828 = CARTESIAN_POINT ( 'NONE',  ( 41.46631938032478359, 75.38445800887258486, 38.96596240072933170 ) ) ;
#6829 = CARTESIAN_POINT ( 'NONE',  ( -88.69383338279318707, 132.1114735047150646, -25.00000000000000000 ) ) ;
#6830 = CARTESIAN_POINT ( 'NONE',  ( 38.96631938032478359, 129.4104996726487684, 31.27175355779120025 ) ) ;
#6832 = CARTESIAN_POINT ( 'NONE',  ( 74.63589561985200760, 132.8035080205385157, -14.84689682711585768 ) ) ;
#6831 = CARTESIAN_POINT ( 'NONE',  ( 40.27526882409969033, 83.66518717409398675, 30.44471234641811819 ) ) ;
#6833 =( BOUNDED_SURFACE ( )  B_SPLINE_SURFACE ( 1, 2, ( 
 ( #9637, #16337, #7980, #14687, #6316, #20109, #8635, #4999, #18332, #14902, #15245, #6773, #18660, #248, #1801, #18554, #11930, #1469, #16554, #6665, #6986, #13689, #5320, #1900, #15356, #20423, #13481, #18767, #13372, #11709, #143, #15016, #8533, #3232, #21755, #3343, #12034, #16992, #3563, #18445, #3460, #10288, #20213, #8420, #5106, #9965, #6541, #19999, #16780, #10071, #9852, #20318, #6874, #15130, #21650, #8201, #1691, #13581, #13262, #11822, #33, #5217, #10184, #4883, #11602, #16668, #1579, #8308, #16884, #3993, #5521, #679, #5419, #17421, #18869, #20639, #10609, #5633, #3777, #10506, #17202, #788, #12251, #2117, #17527, #15662, #2014, #10398, #17314, #12357, #18982, #15560, #19198, #5849, #12136, #9177, #8854, #7416, #15874, #2437, #7310, #12579, #7196, #3884, #9066, #464, #2327, #13900, #2225, #8956, #7523, #10828, #12467, #565, #19094, #4095, #14011, #20744, #10718, #15774, #362, #13794, #14116, #20854, #5743, #14224, #20964, #3668, #15462, #17098, #8745, #7090, #20532, #14552, #2648, #14659, #19515, #16311, #2545, #7632, #17964, #2981, #18074, #19629, #21177, #1222, #21076, #11244, #12684, #14443, #4407, #21294, #19407, #4305, #11030, #16420, #6068, #17743, #11351, #9505, #17638, #4202, #11139, #6172, #12795, #9390, #13019, #21514, #5958, #9719, #16096, #7955, #1006, #1331, #17854, #6288, #19739, #2765, #8064, #893, #10930, #15983, #14771, #4522, #16202, #1114, #21401, #7849, #12906, #2869, #9613, #7742, #6399, #4632, #19304, #9282, #14336, #4740, #6513, #11576, #13556, #1772, #16752, #20291, #14878, #13127, #3206, #1553, #11905, #8284, #21623, #18188, #18527, #10048, #118, #3538, #5082, #7, #15218, #11459, #19849, #9937, #10263, #16965, #8608, #5187, #8395, #18304, #8506, #13348, #10157, #3096, #1444, #11796, #18634, #1877, #13455, #14984, #16858, #13234, #3435, #19972, #21730, #20085, #15103, #4857, #16643, #6637, #15329, #4972, #11684, #221, #3319, #9827, #16525, #18421, #6748, #1661, #20189, #6849, #8173, #15436, #12444, #7063, #10692, #13767, #19171, #13875, #15752, #655, #12226, #5720, #10371, #13665, #3644, #2414, #7284, #2094, #10585, #17398, #442, #20614, #543, #13984, #5396, #9153, #14092, #20721, #9042, #17288, #20398, #335, #12114, #7392, #2301, #2202, #20828, #8718, #6957, #18845, #17181, #4071, #8828, #20509, #12006, #12331, #3860, #10800, #17504, #5606, #15638, #15851, #5293, #18741, #3752, #17072, #1985, #10480, #15536, #7172, #5498, #8932, #18958, #19067, #3969, #2738, #7606, #11113, #17612, #14308, #4277, #18251, #12878, #14525, #21051, #6040, #21265, #14418, #9363, #21154, #2518, #12553, #4179, #17716, #5932, #7821, #16177, #9477, #16066, #5821, #9883, #2622, #17828, #19279, #19489, #12662, #7717, #1088, #11006, #977, #12768, #4381, #871, #16581, #19598, #6144, #4492, #11216, #14201, #9258, #19383, #3151, #1500, #762, #7499, #15958, #20939, #10909, #8896, #19237, #15597, #7132, #3708, #4030, #17356, #7453, #10868, #12400, #7349, #723, #12074, #5358, #17245, #17570, #2477, #15916, #12511, #4137, #9218, #2261, #7563, #2159, #503, #10756, #3816, #19132, #13836, #10545, #13942, #829, #5780, #14160, #7240, #14053, #20893, #8998, #19025, #15707, #20572, #17140, #8786, #5565, #20680, #20465, #9110, #17462, #3923, #10440, #18805, #12287, #2373, #2054, #613, #10654, #15810, #20785, #15500, #402, #5458, #12180, #18915, #5676, #14893, #16434, #11593, #16326, #6532, #7970, #9737, #21528, #16543, #14676, #21417, #6305, #11699, #1348, #13033, #6654, #4757, #12921, #21007, #6418, #1459, #8080, #4651, #8298, #16769, #1235, #20100, #19757, #18321, #11370, #4989, #13141, #1570, #15005, #19870, #13362, #17978, #6190, #11257, #10062, #21746, #16658, #14786, #21641, #3334, #18434, #11476, #18204, #1681, #3111, #19646, #18091, #13251, #2999, #14261, #9843, #8192, #19988, #4873, #3222, #9954, #4537, #2890, #9627, #3768, #10495, #18973, #10388, #5512, #11813, #10174, #15553, #1890, #3552, #18758, #8734, #17196, #12243, #15119, #11921, #17305, #20630, #18650, #16874, #1790, #456, #5410, #3876, #10278, #10601, #6864, #8410, #22, #134, #2109, #12128, #8846, #20523, #6762, #18544, #7187, #13471, #20203, #18861, #13784, #8522, #236, #13893, #6976, #5096, #3450, #15235, #13569, #13680, #20414, #20307, #5205, #16981, #8626, #15344, #5310, #12022, #3658, #17089, #2003, #15453, #352, #9380, #16084, #21067, #17732, #17629, #2638, #19504, #20736, #5625, #14434, #995, #14002, #885, #7733, #4397, #5948, #21168, #7407, #3985, #7624, #12349, #15767, #15654, #14107, #19085, #14325, #10710, #12784, #9273, #6058, #11130, #19398, #19189, #671, #15974, #2217, #4294, #4087, #8947, #17413, #14215, #9057, #20845, #12459, #10818, #9169, #10922, #17519, #2430, #780, #7515, #20954, #5838, #12569, #19296, #16192, #2753, #2970, #4730, #13008, #7942, #11565, #20075, #4510, #1541, #17952, #21612, #2858, #8273, #9709, #4844, #18294, #1320, #16631, #21281, #9494, #14540, #13337, #18177, #19728, #21501, #6502, #11341, #16411, #11449, #3083, #16301, #4961, #3196, #9817, #19960, #6388, #1103, #11232, #1209, #9926, #13222, #13116, #14973, #19615 ),
 ( #21719, #16515, #4621, #17845, #6622, #8053, #7838, #6160, #18064, #1432, #12895, #9601, #14759, #19839, #14649, #8161, #21389, #6276, #14866, #1761, #2085, #10145, #3528, #13653, #18513, #1867, #20387, #16740, #11784, #18731, #7054, #13759, #432, #5284, #8817, #15092, #13444, #18836, #5175, #6839, #210, #11998, #20499, #15527, #18407, #15207, #20603, #7163, #107, #20179, #11894, #18623, #3636, #10361, #16846, #13866, #3742, #17062, #5388, #15316, #3307, #5070, #8495, #12104, #323, #6947, #10471, #3424, #11672, #13545, #20281, #17172, #10253, #16955, #1652, #1974, #8597, #10035, #8383, #8709, #15428, #4939, #6737, #12214, #2290, #2613, #9351, #967, #19375, #10998, #4270, #9142, #14407, #9030, #7381, #10899, #10681, #19270, #13973, #17386, #20819, #16055, #12651, #14296, #15741, #14190, #21040, #15842, #4060, #753, #20711, #2191, #15627, #12434, #646, #7596, #15949, #2509, #10789, #17276, #7708, #19161, #17603, #8922, #7488, #14082, #860, #5710, #9250, #10575, #532, #4170, #5487, #3849, #5811, #17495, #5923, #7271, #5594, #12321, #2406, #20929, #12542, #19056, #3958, #6136, #18265, #7918, #14516, #13194, #11312, #19480, #6029, #6249, #8028, #16278, #11207, #14836, #1516, #7810, #4815, #21256, #3054, #12866, #11538, #12979, #8133, #21583, #4594, #19927, #2727, #12759, #17815, #16600, #21471, #1184, #2942, #9793, #19587, #16487, #4480, #3169, #19703, #6473, #9898, #18037, #8245, #9468, #4371, #16167, #21144, #6362, #14621, #9684, #1404, #21358, #16381, #14735, #13086, #17924, #11102, #1079, #19814, #2833, #1293, #9572, #4703, #11421, #18147, #3612, #18600, #300, #16713, #14947, #5044, #3392, #13734, #10116, #1622, #20048, #20364, #11868, #1950, #5364, #6921, #1845, #17038, #6593, #21694, #11755, #12081, #18811, #10445, #7029, #20472, #3716, #3504, #2062, #18486, #16823, #5259, #20152, #13625, #8354, #1735, #8470, #17147, #13312, #8680, #15178, #8575, #15402, #10227, #13523, #16929, #15065, #11645, #3278, #80, #6817, #4935, #10335, #11976, #20257, #18377, #10008, #5148, #18706, #21802, #15291, #184, #6709, #13417, #5787, #13842, #18921, #7458, #14269, #7569, #9118, #10660, #12519, #10550, #730, #2164, #3929, #15716, #10764, #8901, #15603, #510, #5896, #17362, #7248, #835, #20791, #7138, #15506, #620, #17470, #2268, #20686, #2483, #10972, #17251, #21014, #12626, #19243, #9005, #13948, #15816, #9225, #14167, #7355, #17684, #19348, #5683, #15923, #10876, #14058, #20900, #4246, #8792, #12407, #19138, #17577, #4037, #408, #5570, #4143, #12293, #20578, #19031, #2380, #5464, #12186, #3824, #4568, #7684, #2697, #9657, #19789, #4681, #13170, #11290, #21558, #6004, #4346, #9767, #17897, #19558, #12953, #2922, #11396, #6448, #9327, #6110, #11510, #14813, #12840, #11074, #17789, #16464, #21446, #19902, #4453, #4790, #1051, #2587, #16026, #16142, #18120, #6336, #3030, #14710, #939, #12733, #1378, #14381, #21120, #13061, #1268, #9442, #16251, #8107, #1160, #19456, #7785, #14489, #21231, #7893, #14594, #11184, #2810, #9548, #21335, #6222, #19676, #18011, #16357, #8003, #5337, #3480, #8221, #3583, #10311, #15265, #5234, #11844, #11951, #13709, #14922, #21671, #8656, #18681, #6566, #16907, #17013, #20445, #162, #1920, #1596, #20021, #1819, #13286, #9984, #9872, #8329, #1491, #8553, #4907, #7005, #18573, #15378, #271, #13602, #15038, #18240, #21779, #3142, #6685, #6894, #16572, #11623, #10204, #18351, #3255, #16688, #20339, #13393, #20127, #5021, #11730, #18463, #3366, #10091, #16798, #1711, #8445, #15151, #52, #6794, #13501, #20233, #5126, #17440, #381, #3798, #3688, #17224, #17121, #2351, #13815, #807, #12380, #9197, #2457, #9088, #7220, #10526, #19115, #5762, #4010, #13921, #20986, #15895, #2244, #12490, #14137, #20661, #10738, #7544, #17547, #5542, #8978, #20874, #12269, #10416, #18891, #15791, #2140, #14243, #8873, #3907, #14031, #15580, #15684, #20766, #2033, #12159, #700, #7434, #19217, #12054, #5657, #18785, #15480, #20555, #4115, #19005, #10634, #591, #10851, #8765, #7110, #5438, #483, #17337, #7331, #9412, #7659, #21097, #13038, #2897, #3004, #7763, #9742, #4324, #16439, #1353, #19430, #1241, #9632, #7975, #17983, #8084, #9302, #14682, #14791, #17659, #16331, #4542, #5980, #19533, #21422, #4427, #6311, #19762, #4659, #11374, #11159, #17872, #16003, #11264, #18095, #5872, #6195, #14460, #12601, #14356, #19651, #12706, #1026, #12814, #7868, #11049, #17764, #2668, #19323, #21202, #16120, #4222, #2783, #10951, #2564, #9525, #14568, #6086, #16223, #913, #1134, #21310, #12926, #21645, #3455, #6536, #5211, #6659, #8527, #15240, #4993, #20312, #3116, #6423, #18210, #17283, #28, #16662, #3338, #10178, #15009, #13367, #15123, #6766, #19993, #2198, #6868, #13475, #1796, #10066, #13145, #14897, #4878, #138, #16879, #16773, #13575, #1464, #21533, #11597, #9960, #12220, #1574, #8196, #4761, #5101, #18439, #18954, #3857, #20207, #8415, #10580, #19874, #11480, #18327, #8928, #9847, #16548, #13256, #3226, #8302, #1685, #21750, #20104, #11703, #11817, #18548, #7601, #2296, #5715, #9148, #12764, #972, #2618, #12440, #2514, #9357, #4176, #14196 ) ),
 .UNSPECIFIED., .F., .F., .T. ) 
 B_SPLINE_SURFACE_WITH_KNOTS ( ( 2, 2 ),
 ( 3, 2, 2, 2, 2, 2, 2, 2, 2, 2, 2, 2, 2, 2, 2, 2, 2, 2, 2, 2, 2, 2, 2, 2, 2, 2, 2, 2, 2, 2, 2, 2, 2, 2, 2, 2, 2, 2, 2, 2, 2, 2, 2, 2, 2, 2, 2, 2, 2, 2, 2, 2, 2, 2, 2, 2, 2, 2, 2, 2, 2, 2, 2, 2, 2, 2, 2, 2, 2, 2, 2, 2, 2, 2, 2, 2, 2, 2, 2, 2, 2, 2, 2, 2, 2, 2, 2, 2, 2, 2, 2, 2, 2, 2, 2, 2, 2, 2, 2, 2, 2, 2, 2, 2, 2, 2, 2, 2, 2, 2, 2, 2, 2, 2, 2, 2, 2, 2, 2, 2, 2, 2, 2, 2, 2, 2, 2, 2, 2, 2, 2, 2, 2, 2, 2, 2, 2, 2, 2, 2, 2, 2, 2, 2, 2, 2, 2, 2, 2, 2, 2, 2, 2, 2, 2, 2, 2, 2, 2, 2, 2, 2, 2, 2, 2, 2, 2, 2, 2, 2, 2, 2, 2, 2, 2, 2, 2, 2, 2, 2, 2, 2, 2, 2, 2, 2, 2, 2, 2, 2, 2, 2, 2, 2, 2, 2, 2, 2, 2, 2, 2, 2, 2, 2, 2, 2, 2, 2, 2, 2, 2, 2, 2, 2, 2, 2, 2, 2, 2, 2, 2, 2, 2, 2, 2, 2, 2, 2, 2, 2, 2, 2, 2, 2, 2, 2, 2, 2, 2, 2, 2, 2, 2, 2, 2, 2, 2, 2, 2, 2, 2, 2, 2, 2, 2, 2, 2, 2, 2, 2, 2, 2, 2, 2, 2, 2, 2, 2, 2, 2, 2, 2, 2, 2, 2, 2, 2, 2, 2, 2, 2, 2, 2, 2, 2, 2, 2, 2, 2, 2, 2, 2, 2, 2, 2, 2, 2, 2, 2, 2, 2, 2, 2, 2, 2, 2, 2, 2, 2, 2, 2, 2, 2, 2, 2, 2, 2, 2, 2, 2, 2, 2, 2, 2, 2, 2, 2, 2, 2, 2, 2, 2, 2, 2, 3 ),
 ( 0.000000000000000000, 1.000000000000000000 ),
 ( 0.000000000000000000, 0.002941176470588235253, 0.005882352941176470507, 0.008823529411764705760, 0.01176470588235294101, 0.01470588235294117627, 0.01764705882352941152, 0.02058823529411764677, 0.02352941176470588203, 0.02647058823529411728, 0.02941176470588235253, 0.03235294117647059126, 0.03529411764705882304, 0.03823529411764706176, 0.04117647058823529355, 0.04411764705882353227, 0.04705882352941176405, 0.05000000000000000278, 0.05294117647058823456, 0.05588235294117647328, 0.05882352941176470507, 0.06176470588235294379, 0.06470588235294118251, 0.06764705882352940736, 0.07058823529411764608, 0.07352941176470588480, 0.07647058823529412352, 0.07941176470588234837, 0.08235294117647058709, 0.08529411764705882582, 0.08823529411764706454, 0.09117647058823528938, 0.09411764705882352811, 0.09705882352941176683, 0.1000000000000000056, 0.1029411764705882304, 0.1058823529411764691, 0.1088235294117647078, 0.1117647058823529466, 0.1147058823529411714, 0.1176470588235294101, 0.1205882352941176489, 0.1235294117647058876, 0.1264705882352941124, 0.1294117647058823650, 0.1323529411764705899, 0.1352941176470588147, 0.1382352941176470673, 0.1411764705882352922, 0.1441176470588235170, 0.1470588235294117696, 0.1499999999999999944, 0.1529411764705882470, 0.1558823529411764719, 0.1588235294117646967, 0.1617647058823529493, 0.1647058823529411742, 0.1676470588235293990, 0.1705882352941176516, 0.1735294117647058765, 0.1764705882352941291, 0.1794117647058823539, 0.1823529411764705788, 0.1852941176470588314, 0.1882352941176470562, 0.1911764705882352811, 0.1941176470588235337, 0.1970588235294117585, 0.2000000000000000111, 0.2029411764705882359, 0.2058823529411764608, 0.2088235294117647134, 0.2117647058823529382, 0.2147058823529411631, 0.2176470588235294157, 0.2205882352941176405, 0.2235294117647058931, 0.2264705882352941180, 0.2294117647058823428, 0.2323529411764705954, 0.2352941176470588203, 0.2382352941176470451, 0.2411764705882352977, 0.2441176470588235226, 0.2470588235294117752, 0.2500000000000000000, 0.2529411764705882248, 0.2558823529411764497, 0.2588235294117647300, 0.2617647058823529549, 0.2647058823529411797, 0.2676470588235294046, 0.2705882352941176294, 0.2735294117647059098, 0.2764705882352941346, 0.2794117647058823595, 0.2823529411764705843, 0.2852941176470588092, 0.2882352941176470340, 0.2911764705882353144, 0.2941176470588235392, 0.2970588235294117641, 0.2999999999999999889, 0.3029411764705882137, 0.3058823529411764941, 0.3088235294117647189, 0.3117647058823529438, 0.3147058823529411686, 0.3176470588235293935, 0.3205882352941176738, 0.3235294117647058987, 0.3264705882352941235, 0.3294117647058823484, 0.3323529411764705732, 0.3352941176470587981, 0.3382352941176470784, 0.3411764705882353033, 0.3441176470588235281, 0.3470588235294117530, 0.3499999999999999778, 0.3529411764705882582, 0.3558823529411764830, 0.3588235294117647078, 0.3617647058823529327, 0.3647058823529411575, 0.3676470588235294379, 0.3705882352941176627, 0.3735294117647058876, 0.3764705882352941124, 0.3794117647058823373, 0.3823529411764705621, 0.3852941176470588425, 0.3882352941176470673, 0.3911764705882352922, 0.3941176470588235170, 0.3970588235294117418, 0.4000000000000000222, 0.4029411764705882470, 0.4058823529411764719, 0.4088235294117646967, 0.4117647058823529216, 0.4147058823529412019, 0.4176470588235294268, 0.4205882352941176516, 0.4235294117647058765, 0.4264705882352941013, 0.4294117647058823262, 0.4323529411764706065, 0.4352941176470588314, 0.4382352941176470562, 0.4411764705882352811, 0.4441176470588235059, 0.4470588235294117863, 0.4500000000000000111, 0.4529411764705882359, 0.4558823529411764608, 0.4588235294117646856, 0.4617647058823529660, 0.4647058823529411908, 0.4676470588235294157, 0.4705882352941176405, 0.4735294117647058654, 0.4764705882352940902, 0.4794117647058823706, 0.4823529411764705954, 0.4852941176470588203, 0.4882352941176470451, 0.4911764705882352700, 0.4941176470588235503, 0.4970588235294117752, 0.5000000000000000000, 0.5029411764705882248, 0.5058823529411764497, 0.5088235294117646745, 0.5117647058823528994, 0.5147058823529411242, 0.5176470588235294601, 0.5205882352941176849, 0.5235294117647059098, 0.5264705882352941346, 0.5294117647058823595, 0.5323529411764705843, 0.5352941176470588092, 0.5382352941176470340, 0.5411764705882352589, 0.5441176470588234837, 0.5470588235294118196, 0.5500000000000000444, 0.5529411764705882693, 0.5558823529411764941, 0.5588235294117647189, 0.5617647058823529438, 0.5647058823529411686, 0.5676470588235293935, 0.5705882352941176183, 0.5735294117647058432, 0.5764705882352940680, 0.5794117647058824039, 0.5823529411764706287, 0.5852941176470588536, 0.5882352941176470784, 0.5911764705882353033, 0.5941176470588235281, 0.5970588235294117530, 0.5999999999999999778, 0.6029411764705882026, 0.6058823529411764275, 0.6088235294117646523, 0.6117647058823529882, 0.6147058823529412130, 0.6176470588235294379, 0.6205882352941176627, 0.6235294117647058876, 0.6264705882352941124, 0.6294117647058823373, 0.6323529411764705621, 0.6352941176470587870, 0.6382352941176470118, 0.6411764705882353477, 0.6441176470588235725, 0.6470588235294117974, 0.6500000000000000222, 0.6529411764705882470, 0.6558823529411764719, 0.6588235294117646967, 0.6617647058823529216, 0.6647058823529411464, 0.6676470588235293713, 0.6705882352941175961, 0.6735294117647059320, 0.6764705882352941568, 0.6794117647058823817, 0.6823529411764706065, 0.6852941176470588314, 0.6882352941176470562, 0.6911764705882352811, 0.6941176470588235059, 0.6970588235294117307, 0.6999999999999999556, 0.7029411764705881804, 0.7058823529411765163, 0.7088235294117647411, 0.7117647058823529660, 0.7147058823529411908, 0.7176470588235294157, 0.7205882352941176405, 0.7235294117647058654, 0.7264705882352940902, 0.7294117647058823151, 0.7323529411764705399, 0.7352941176470588758, 0.7382352941176471006, 0.7411764705882353255, 0.7441176470588235503, 0.7470588235294117752, 0.7500000000000000000, 0.7529411764705882248, 0.7558823529411764497, 0.7588235294117646745, 0.7617647058823528994, 0.7647058823529411242, 0.7676470588235294601, 0.7705882352941176849, 0.7735294117647059098, 0.7764705882352941346, 0.7794117647058823595, 0.7823529411764705843, 0.7852941176470588092, 0.7882352941176470340, 0.7911764705882352589, 0.7941176470588234837, 0.7970588235294118196, 0.8000000000000000444, 0.8029411764705882693, 0.8058823529411764941, 0.8088235294117647189, 0.8117647058823529438, 0.8147058823529411686, 0.8176470588235293935, 0.8205882352941176183, 0.8235294117647058432, 0.8264705882352940680, 0.8294117647058824039, 0.8323529411764706287, 0.8352941176470588536, 0.8382352941176470784, 0.8411764705882353033, 0.8441176470588235281, 0.8470588235294117530, 0.8499999999999999778, 0.8529411764705882026, 0.8558823529411764275, 0.8588235294117646523, 0.8617647058823529882, 0.8647058823529412130, 0.8676470588235294379, 0.8705882352941176627, 0.8735294117647058876, 0.8764705882352941124, 0.8794117647058823373, 0.8823529411764705621, 0.8852941176470587870, 0.8882352941176470118, 0.8911764705882353477, 0.8941176470588235725, 0.8970588235294117974, 0.9000000000000000222, 0.9029411764705882470, 0.9058823529411764719, 0.9088235294117646967, 0.9117647058823529216, 0.9147058823529411464, 0.9176470588235293713, 0.9205882352941175961, 0.9235294117647059320, 0.9264705882352941568, 0.9294117647058823817, 0.9323529411764706065, 0.9352941176470588314, 0.9382352941176470562, 0.9411764705882352811, 0.9441176470588235059, 0.9470588235294117307, 0.9499999999999999556, 0.9529411764705881804, 0.9558823529411765163, 0.9588235294117647411, 0.9617647058823529660, 0.9647058823529411908, 0.9676470588235294157, 0.9705882352941176405, 0.9735294117647058654, 0.9764705882352940902, 0.9794117647058823151, 0.9803958342062288889 ),
 .UNSPECIFIED. ) 
 GEOMETRIC_REPRESENTATION_ITEM ( )  RATIONAL_B_SPLINE_SURFACE ( (
 ( 1.000000000000000000, 0.9510565162951535312, 1.000000000000000000, 0.9510565162951535312, 1.000000000000000000, 0.9510565162951535312, 1.000000000000000000, 0.9510565162951535312, 1.000000000000000000, 0.9510565162951535312, 1.000000000000000000, 0.9510565162951535312, 1.000000000000000000, 0.9510565162951535312, 1.000000000000000000, 0.9510565162951535312, 1.000000000000000000, 0.9510565162951535312, 1.000000000000000000, 0.9510565162951535312, 1.000000000000000000, 0.9510565162951535312, 1.000000000000000000, 0.9510565162951535312, 1.000000000000000000, 0.9510565162951535312, 1.000000000000000000, 0.9510565162951535312, 1.000000000000000000, 0.9510565162951535312, 1.000000000000000000, 0.9510565162951535312, 1.000000000000000000, 0.9510565162951535312, 1.000000000000000000, 0.9510565162951535312, 1.000000000000000000, 0.9510565162951535312, 1.000000000000000000, 0.9510565162951535312, 1.000000000000000000, 0.9510565162951535312, 1.000000000000000000, 0.9510565162951535312, 1.000000000000000000, 0.9510565162951535312, 1.000000000000000000, 0.9510565162951535312, 1.000000000000000000, 0.9510565162951535312, 1.000000000000000000, 0.9510565162951535312, 1.000000000000000000, 0.9510565162951535312, 1.000000000000000000, 0.9510565162951535312, 1.000000000000000000, 0.9510565162951535312, 1.000000000000000000, 0.9510565162951535312, 1.000000000000000000, 0.9510565162951535312, 1.000000000000000000, 0.9510565162951535312, 1.000000000000000000, 0.9510565162951535312, 1.000000000000000000, 0.9510565162951535312, 1.000000000000000000, 0.9510565162951535312, 1.000000000000000000, 0.9510565162951535312, 1.000000000000000000, 0.9510565162951535312, 1.000000000000000000, 0.9510565162951535312, 1.000000000000000000, 0.9510565162951535312, 1.000000000000000000, 0.9510565162951535312, 1.000000000000000000, 0.9510565162951535312, 1.000000000000000000, 0.9510565162951535312, 1.000000000000000000, 0.9510565162951535312, 1.000000000000000000, 0.9510565162951535312, 1.000000000000000000, 0.9510565162951535312, 1.000000000000000000, 0.9510565162951535312, 1.000000000000000000, 0.9510565162951535312, 1.000000000000000000, 0.9510565162951535312, 1.000000000000000000, 0.9510565162951535312, 1.000000000000000000, 0.9510565162951535312, 1.000000000000000000, 0.9510565162951535312, 1.000000000000000000, 0.9510565162951535312, 1.000000000000000000, 0.9510565162951535312, 1.000000000000000000, 0.9510565162951535312, 1.000000000000000000, 0.9510565162951535312, 1.000000000000000000, 0.9510565162951535312, 1.000000000000000000, 0.9510565162951535312, 1.000000000000000000, 0.9510565162951535312, 1.000000000000000000, 0.9510565162951535312, 1.000000000000000000, 0.9510565162951535312, 1.000000000000000000, 0.9510565162951535312, 1.000000000000000000, 0.9510565162951535312, 1.000000000000000000, 0.9510565162951535312, 1.000000000000000000, 0.9510565162951535312, 1.000000000000000000, 0.9510565162951535312, 1.000000000000000000, 0.9510565162951535312, 1.000000000000000000, 0.9510565162951535312, 1.000000000000000000, 0.9510565162951535312, 1.000000000000000000, 0.9510565162951535312, 1.000000000000000000, 0.9510565162951535312, 1.000000000000000000, 0.9510565162951535312, 1.000000000000000000, 0.9510565162951535312, 1.000000000000000000, 0.9510565162951535312, 1.000000000000000000, 0.9510565162951535312, 1.000000000000000000, 0.9510565162951535312, 1.000000000000000000, 0.9510565162951535312, 1.000000000000000000, 0.9510565162951535312, 1.000000000000000000, 0.9510565162951535312, 1.000000000000000000, 0.9510565162951535312, 1.000000000000000000, 0.9510565162951535312, 1.000000000000000000, 0.9510565162951535312, 1.000000000000000000, 0.9510565162951535312, 1.000000000000000000, 0.9510565162951535312, 1.000000000000000000, 0.9510565162951535312, 1.000000000000000000, 0.9510565162951535312, 1.000000000000000000, 0.9510565162951535312, 1.000000000000000000, 0.9510565162951535312, 1.000000000000000000, 0.9510565162951535312, 1.000000000000000000, 0.9510565162951535312, 1.000000000000000000, 0.9510565162951535312, 1.000000000000000000, 0.9510565162951535312, 1.000000000000000000, 0.9510565162951535312, 1.000000000000000000, 0.9510565162951535312, 1.000000000000000000, 0.9510565162951535312, 1.000000000000000000, 0.9510565162951535312, 1.000000000000000000, 0.9510565162951535312, 1.000000000000000000, 0.9510565162951535312, 1.000000000000000000, 0.9510565162951535312, 1.000000000000000000, 0.9510565162951535312, 1.000000000000000000, 0.9510565162951535312, 1.000000000000000000, 0.9510565162951535312, 1.000000000000000000, 0.9510565162951535312, 1.000000000000000000, 0.9510565162951535312, 1.000000000000000000, 0.9510565162951535312, 1.000000000000000000, 0.9510565162951535312, 1.000000000000000000, 0.9510565162951535312, 1.000000000000000000, 0.9510565162951535312, 1.000000000000000000, 0.9510565162951535312, 1.000000000000000000, 0.9510565162951535312, 1.000000000000000000, 0.9510565162951535312, 1.000000000000000000, 0.9510565162951535312, 1.000000000000000000, 0.9510565162951535312, 1.000000000000000000, 0.9510565162951535312, 1.000000000000000000, 0.9510565162951535312, 1.000000000000000000, 0.9510565162951535312, 1.000000000000000000, 0.9510565162951535312, 1.000000000000000000, 0.9510565162951535312, 1.000000000000000000, 0.9510565162951535312, 1.000000000000000000, 0.9510565162951535312, 1.000000000000000000, 0.9510565162951535312, 1.000000000000000000, 0.9510565162951535312, 1.000000000000000000, 0.9510565162951535312, 1.000000000000000000, 0.9510565162951535312, 1.000000000000000000, 0.9510565162951535312, 1.000000000000000000, 0.9510565162951535312, 1.000000000000000000, 0.9510565162951535312, 1.000000000000000000, 0.9510565162951535312, 1.000000000000000000, 0.9510565162951535312, 1.000000000000000000, 0.9510565162951535312, 1.000000000000000000, 0.9510565162951535312, 1.000000000000000000, 0.9510565162951535312, 1.000000000000000000, 0.9510565162951535312, 1.000000000000000000, 0.9510565162951535312, 1.000000000000000000, 0.9510565162951535312, 1.000000000000000000, 0.9510565162951535312, 1.000000000000000000, 0.9510565162951535312, 1.000000000000000000, 0.9510565162951535312, 1.000000000000000000, 0.9510565162951535312, 1.000000000000000000, 0.9510565162951535312, 1.000000000000000000, 0.9510565162951535312, 1.000000000000000000, 0.9510565162951535312, 1.000000000000000000, 0.9510565162951535312, 1.000000000000000000, 0.9510565162951535312, 1.000000000000000000, 0.9510565162951535312, 1.000000000000000000, 0.9510565162951535312, 1.000000000000000000, 0.9510565162951535312, 1.000000000000000000, 0.9510565162951535312, 1.000000000000000000, 0.9510565162951535312, 1.000000000000000000, 0.9510565162951535312, 1.000000000000000000, 0.9510565162951535312, 1.000000000000000000, 0.9510565162951535312, 1.000000000000000000, 0.9510565162951535312, 1.000000000000000000, 0.9510565162951535312, 1.000000000000000000, 0.9510565162951535312, 1.000000000000000000, 0.9510565162951535312, 1.000000000000000000, 0.9510565162951535312, 1.000000000000000000, 0.9510565162951535312, 1.000000000000000000, 0.9510565162951535312, 1.000000000000000000, 0.9510565162951535312, 1.000000000000000000, 0.9510565162951535312, 1.000000000000000000, 0.9510565162951535312, 1.000000000000000000, 0.9510565162951535312, 1.000000000000000000, 0.9510565162951535312, 1.000000000000000000, 0.9510565162951535312, 1.000000000000000000, 0.9510565162951535312, 1.000000000000000000, 0.9510565162951535312, 1.000000000000000000, 0.9510565162951535312, 1.000000000000000000, 0.9510565162951535312, 1.000000000000000000, 0.9510565162951535312, 1.000000000000000000, 0.9510565162951535312, 1.000000000000000000, 0.9510565162951535312, 1.000000000000000000, 0.9510565162951535312, 1.000000000000000000, 0.9510565162951535312, 1.000000000000000000, 0.9510565162951535312, 1.000000000000000000, 0.9510565162951535312, 1.000000000000000000, 0.9510565162951535312, 1.000000000000000000, 0.9510565162951535312, 1.000000000000000000, 0.9510565162951535312, 1.000000000000000000, 0.9510565162951535312, 1.000000000000000000, 0.9510565162951535312, 1.000000000000000000, 0.9510565162951535312, 1.000000000000000000, 0.9510565162951535312, 1.000000000000000000, 0.9510565162951535312, 1.000000000000000000, 0.9510565162951535312, 1.000000000000000000, 0.9510565162951535312, 1.000000000000000000, 0.9510565162951535312, 1.000000000000000000, 0.9510565162951535312, 1.000000000000000000, 0.9510565162951535312, 1.000000000000000000, 0.9510565162951535312, 1.000000000000000000, 0.9510565162951535312, 1.000000000000000000, 0.9510565162951535312, 1.000000000000000000, 0.9510565162951535312, 1.000000000000000000, 0.9510565162951535312, 1.000000000000000000, 0.9510565162951535312, 1.000000000000000000, 0.9510565162951535312, 1.000000000000000000, 0.9510565162951535312, 1.000000000000000000, 0.9510565162951535312, 1.000000000000000000, 0.9510565162951535312, 1.000000000000000000, 0.9510565162951535312, 1.000000000000000000, 0.9510565162951535312, 1.000000000000000000, 0.9510565162951535312, 1.000000000000000000, 0.9510565162951535312, 1.000000000000000000, 0.9510565162951535312, 1.000000000000000000, 0.9510565162951535312, 1.000000000000000000, 0.9510565162951535312, 1.000000000000000000, 0.9510565162951535312, 1.000000000000000000, 0.9510565162951535312, 1.000000000000000000, 0.9510565162951535312, 1.000000000000000000, 0.9510565162951535312, 1.000000000000000000, 0.9510565162951535312, 1.000000000000000000, 0.9510565162951535312, 1.000000000000000000, 0.9510565162951535312, 1.000000000000000000, 0.9510565162951535312, 1.000000000000000000, 0.9510565162951535312, 1.000000000000000000, 0.9510565162951535312, 1.000000000000000000, 0.9510565162951535312, 1.000000000000000000, 0.9510565162951535312, 1.000000000000000000, 0.9510565162951535312, 1.000000000000000000, 0.9510565162951535312, 1.000000000000000000, 0.9510565162951535312, 1.000000000000000000, 0.9510565162951535312, 1.000000000000000000, 0.9510565162951535312, 1.000000000000000000, 0.9510565162951535312, 1.000000000000000000, 0.9510565162951535312, 1.000000000000000000, 0.9510565162951535312, 1.000000000000000000, 0.9510565162951535312, 1.000000000000000000, 0.9510565162951535312, 1.000000000000000000, 0.9510565162951535312, 1.000000000000000000, 0.9510565162951535312, 1.000000000000000000, 0.9510565162951535312, 1.000000000000000000, 0.9510565162951535312, 1.000000000000000000, 0.9510565162951535312, 1.000000000000000000, 0.9510565162951535312, 1.000000000000000000, 0.9510565162951535312, 1.000000000000000000, 0.9510565162951535312, 1.000000000000000000, 0.9510565162951535312, 1.000000000000000000, 0.9510565162951535312, 1.000000000000000000, 0.9510565162951535312, 1.000000000000000000, 0.9510565162951535312, 1.000000000000000000, 0.9510565162951535312, 1.000000000000000000, 0.9510565162951535312, 1.000000000000000000, 0.9510565162951535312, 1.000000000000000000, 0.9510565162951535312, 1.000000000000000000, 0.9510565162951535312, 1.000000000000000000, 0.9510565162951535312, 1.000000000000000000, 0.9510565162951535312, 1.000000000000000000, 0.9510565162951535312, 1.000000000000000000, 0.9510565162951535312, 1.000000000000000000, 0.9510565162951535312, 1.000000000000000000, 0.9510565162951535312, 1.000000000000000000, 0.9510565162951535312, 1.000000000000000000, 0.9510565162951535312, 1.000000000000000000, 0.9510565162951535312, 1.000000000000000000, 0.9510565162951535312, 1.000000000000000000, 0.9510565162951535312, 1.000000000000000000, 0.9510565162951535312, 1.000000000000000000, 0.9510565162951535312, 1.000000000000000000, 0.9510565162951535312, 1.000000000000000000, 0.9510565162951535312, 1.000000000000000000, 0.9510565162951535312, 1.000000000000000000, 0.9510565162951535312, 1.000000000000000000, 0.9510565162951535312, 1.000000000000000000, 0.9510565162951535312, 1.000000000000000000, 0.9510565162951535312, 1.000000000000000000, 0.9510565162951535312, 1.000000000000000000, 0.9510565162951535312, 1.000000000000000000, 0.9510565162951535312, 1.000000000000000000, 0.9510565162951535312, 1.000000000000000000, 0.9510565162951535312, 1.000000000000000000, 0.9510565162951535312, 1.000000000000000000, 0.9510565162951535312, 1.000000000000000000, 0.9510565162951535312, 1.000000000000000000, 0.9510565162951535312, 1.000000000000000000, 0.9510565162951535312, 1.000000000000000000, 0.9510565162951535312, 1.000000000000000000, 0.9510565162951535312, 1.000000000000000000, 0.9510565162951535312, 1.000000000000000000, 0.9510565162951535312, 1.000000000000000000, 0.9510565162951535312, 1.000000000000000000, 0.9510565162951535312, 1.000000000000000000, 0.9510565162951535312, 1.000000000000000000, 0.9510565162951535312, 1.000000000000000000, 0.9510565162951535312, 1.000000000000000000, 0.9510565162951535312, 1.000000000000000000, 0.9510565162951535312, 1.000000000000000000, 0.9510565162951535312, 1.000000000000000000, 0.9510565162951535312, 1.000000000000000000, 0.9510565162951535312, 1.000000000000000000, 0.9510565162951535312, 1.000000000000000000, 0.9510565162951535312, 1.000000000000000000, 0.9510565162951535312, 1.000000000000000000, 0.9510565162951535312, 1.000000000000000000, 0.9510565162951535312, 1.000000000000000000, 0.9510565162951535312, 1.000000000000000000, 0.9510565162951535312, 1.000000000000000000, 0.9510565162951535312, 1.000000000000000000, 0.9510565162951535312, 1.000000000000000000, 0.9510565162951535312, 1.000000000000000000, 0.9510565162951535312, 1.000000000000000000, 0.9510565162951535312, 1.000000000000000000, 0.9510565162951535312, 1.000000000000000000, 0.9510565162951535312, 1.000000000000000000, 0.9510565162951535312, 1.000000000000000000, 0.9510565162951535312, 1.000000000000000000, 0.9510565162951535312, 1.000000000000000000, 0.9510565162951535312, 1.000000000000000000, 0.9510565162951535312, 1.000000000000000000, 0.9510565162951535312, 1.000000000000000000, 0.9510565162951535312, 1.000000000000000000, 0.9510565162951535312, 1.000000000000000000, 0.9510565162951535312, 1.000000000000000000, 0.9510565162951535312, 1.000000000000000000, 0.9510565162951535312, 1.000000000000000000, 0.9510565162951535312, 1.000000000000000000, 0.9510565162951535312, 1.000000000000000000, 0.9510565162951535312, 1.000000000000000000, 0.9510565162951535312, 1.000000000000000000, 0.9510565162951535312, 1.000000000000000000, 0.9510565162951535312, 1.000000000000000000, 0.9510565162951535312, 1.000000000000000000, 0.9510565162951535312, 1.000000000000000000, 0.9510565162951535312, 1.000000000000000000, 0.9510565162951535312, 1.000000000000000000, 0.9510565162951535312, 1.000000000000000000, 0.9510565162951535312, 1.000000000000000000, 0.9510565162951535312, 1.000000000000000000, 0.9510565162951535312, 1.000000000000000000, 0.9510565162951535312, 1.000000000000000000, 0.9510565162951535312, 1.000000000000000000, 0.9510565162951535312, 1.000000000000000000, 0.9510565162951535312, 1.000000000000000000, 0.9510565162951535312, 1.000000000000000000, 0.9510565162951535312, 1.000000000000000000, 0.9836243115514193835, 0.9782066976764483002),
 ( 1.000000000000000000, 0.9510565162951535312, 1.000000000000000000, 0.9510565162951535312, 1.000000000000000000, 0.9510565162951535312, 1.000000000000000000, 0.9510565162951535312, 1.000000000000000000, 0.9510565162951535312, 1.000000000000000000, 0.9510565162951535312, 1.000000000000000000, 0.9510565162951535312, 1.000000000000000000, 0.9510565162951535312, 1.000000000000000000, 0.9510565162951535312, 1.000000000000000000, 0.9510565162951535312, 1.000000000000000000, 0.9510565162951535312, 1.000000000000000000, 0.9510565162951535312, 1.000000000000000000, 0.9510565162951535312, 1.000000000000000000, 0.9510565162951535312, 1.000000000000000000, 0.9510565162951535312, 1.000000000000000000, 0.9510565162951535312, 1.000000000000000000, 0.9510565162951535312, 1.000000000000000000, 0.9510565162951535312, 1.000000000000000000, 0.9510565162951535312, 1.000000000000000000, 0.9510565162951535312, 1.000000000000000000, 0.9510565162951535312, 1.000000000000000000, 0.9510565162951535312, 1.000000000000000000, 0.9510565162951535312, 1.000000000000000000, 0.9510565162951535312, 1.000000000000000000, 0.9510565162951535312, 1.000000000000000000, 0.9510565162951535312, 1.000000000000000000, 0.9510565162951535312, 1.000000000000000000, 0.9510565162951535312, 1.000000000000000000, 0.9510565162951535312, 1.000000000000000000, 0.9510565162951535312, 1.000000000000000000, 0.9510565162951535312, 1.000000000000000000, 0.9510565162951535312, 1.000000000000000000, 0.9510565162951535312, 1.000000000000000000, 0.9510565162951535312, 1.000000000000000000, 0.9510565162951535312, 1.000000000000000000, 0.9510565162951535312, 1.000000000000000000, 0.9510565162951535312, 1.000000000000000000, 0.9510565162951535312, 1.000000000000000000, 0.9510565162951535312, 1.000000000000000000, 0.9510565162951535312, 1.000000000000000000, 0.9510565162951535312, 1.000000000000000000, 0.9510565162951535312, 1.000000000000000000, 0.9510565162951535312, 1.000000000000000000, 0.9510565162951535312, 1.000000000000000000, 0.9510565162951535312, 1.000000000000000000, 0.9510565162951535312, 1.000000000000000000, 0.9510565162951535312, 1.000000000000000000, 0.9510565162951535312, 1.000000000000000000, 0.9510565162951535312, 1.000000000000000000, 0.9510565162951535312, 1.000000000000000000, 0.9510565162951535312, 1.000000000000000000, 0.9510565162951535312, 1.000000000000000000, 0.9510565162951535312, 1.000000000000000000, 0.9510565162951535312, 1.000000000000000000, 0.9510565162951535312, 1.000000000000000000, 0.9510565162951535312, 1.000000000000000000, 0.9510565162951535312, 1.000000000000000000, 0.9510565162951535312, 1.000000000000000000, 0.9510565162951535312, 1.000000000000000000, 0.9510565162951535312, 1.000000000000000000, 0.9510565162951535312, 1.000000000000000000, 0.9510565162951535312, 1.000000000000000000, 0.9510565162951535312, 1.000000000000000000, 0.9510565162951535312, 1.000000000000000000, 0.9510565162951535312, 1.000000000000000000, 0.9510565162951535312, 1.000000000000000000, 0.9510565162951535312, 1.000000000000000000, 0.9510565162951535312, 1.000000000000000000, 0.9510565162951535312, 1.000000000000000000, 0.9510565162951535312, 1.000000000000000000, 0.9510565162951535312, 1.000000000000000000, 0.9510565162951535312, 1.000000000000000000, 0.9510565162951535312, 1.000000000000000000, 0.9510565162951535312, 1.000000000000000000, 0.9510565162951535312, 1.000000000000000000, 0.9510565162951535312, 1.000000000000000000, 0.9510565162951535312, 1.000000000000000000, 0.9510565162951535312, 1.000000000000000000, 0.9510565162951535312, 1.000000000000000000, 0.9510565162951535312, 1.000000000000000000, 0.9510565162951535312, 1.000000000000000000, 0.9510565162951535312, 1.000000000000000000, 0.9510565162951535312, 1.000000000000000000, 0.9510565162951535312, 1.000000000000000000, 0.9510565162951535312, 1.000000000000000000, 0.9510565162951535312, 1.000000000000000000, 0.9510565162951535312, 1.000000000000000000, 0.9510565162951535312, 1.000000000000000000, 0.9510565162951535312, 1.000000000000000000, 0.9510565162951535312, 1.000000000000000000, 0.9510565162951535312, 1.000000000000000000, 0.9510565162951535312, 1.000000000000000000, 0.9510565162951535312, 1.000000000000000000, 0.9510565162951535312, 1.000000000000000000, 0.9510565162951535312, 1.000000000000000000, 0.9510565162951535312, 1.000000000000000000, 0.9510565162951535312, 1.000000000000000000, 0.9510565162951535312, 1.000000000000000000, 0.9510565162951535312, 1.000000000000000000, 0.9510565162951535312, 1.000000000000000000, 0.9510565162951535312, 1.000000000000000000, 0.9510565162951535312, 1.000000000000000000, 0.9510565162951535312, 1.000000000000000000, 0.9510565162951535312, 1.000000000000000000, 0.9510565162951535312, 1.000000000000000000, 0.9510565162951535312, 1.000000000000000000, 0.9510565162951535312, 1.000000000000000000, 0.9510565162951535312, 1.000000000000000000, 0.9510565162951535312, 1.000000000000000000, 0.9510565162951535312, 1.000000000000000000, 0.9510565162951535312, 1.000000000000000000, 0.9510565162951535312, 1.000000000000000000, 0.9510565162951535312, 1.000000000000000000, 0.9510565162951535312, 1.000000000000000000, 0.9510565162951535312, 1.000000000000000000, 0.9510565162951535312, 1.000000000000000000, 0.9510565162951535312, 1.000000000000000000, 0.9510565162951535312, 1.000000000000000000, 0.9510565162951535312, 1.000000000000000000, 0.9510565162951535312, 1.000000000000000000, 0.9510565162951535312, 1.000000000000000000, 0.9510565162951535312, 1.000000000000000000, 0.9510565162951535312, 1.000000000000000000, 0.9510565162951535312, 1.000000000000000000, 0.9510565162951535312, 1.000000000000000000, 0.9510565162951535312, 1.000000000000000000, 0.9510565162951535312, 1.000000000000000000, 0.9510565162951535312, 1.000000000000000000, 0.9510565162951535312, 1.000000000000000000, 0.9510565162951535312, 1.000000000000000000, 0.9510565162951535312, 1.000000000000000000, 0.9510565162951535312, 1.000000000000000000, 0.9510565162951535312, 1.000000000000000000, 0.9510565162951535312, 1.000000000000000000, 0.9510565162951535312, 1.000000000000000000, 0.9510565162951535312, 1.000000000000000000, 0.9510565162951535312, 1.000000000000000000, 0.9510565162951535312, 1.000000000000000000, 0.9510565162951535312, 1.000000000000000000, 0.9510565162951535312, 1.000000000000000000, 0.9510565162951535312, 1.000000000000000000, 0.9510565162951535312, 1.000000000000000000, 0.9510565162951535312, 1.000000000000000000, 0.9510565162951535312, 1.000000000000000000, 0.9510565162951535312, 1.000000000000000000, 0.9510565162951535312, 1.000000000000000000, 0.9510565162951535312, 1.000000000000000000, 0.9510565162951535312, 1.000000000000000000, 0.9510565162951535312, 1.000000000000000000, 0.9510565162951535312, 1.000000000000000000, 0.9510565162951535312, 1.000000000000000000, 0.9510565162951535312, 1.000000000000000000, 0.9510565162951535312, 1.000000000000000000, 0.9510565162951535312, 1.000000000000000000, 0.9510565162951535312, 1.000000000000000000, 0.9510565162951535312, 1.000000000000000000, 0.9510565162951535312, 1.000000000000000000, 0.9510565162951535312, 1.000000000000000000, 0.9510565162951535312, 1.000000000000000000, 0.9510565162951535312, 1.000000000000000000, 0.9510565162951535312, 1.000000000000000000, 0.9510565162951535312, 1.000000000000000000, 0.9510565162951535312, 1.000000000000000000, 0.9510565162951535312, 1.000000000000000000, 0.9510565162951535312, 1.000000000000000000, 0.9510565162951535312, 1.000000000000000000, 0.9510565162951535312, 1.000000000000000000, 0.9510565162951535312, 1.000000000000000000, 0.9510565162951535312, 1.000000000000000000, 0.9510565162951535312, 1.000000000000000000, 0.9510565162951535312, 1.000000000000000000, 0.9510565162951535312, 1.000000000000000000, 0.9510565162951535312, 1.000000000000000000, 0.9510565162951535312, 1.000000000000000000, 0.9510565162951535312, 1.000000000000000000, 0.9510565162951535312, 1.000000000000000000, 0.9510565162951535312, 1.000000000000000000, 0.9510565162951535312, 1.000000000000000000, 0.9510565162951535312, 1.000000000000000000, 0.9510565162951535312, 1.000000000000000000, 0.9510565162951535312, 1.000000000000000000, 0.9510565162951535312, 1.000000000000000000, 0.9510565162951535312, 1.000000000000000000, 0.9510565162951535312, 1.000000000000000000, 0.9510565162951535312, 1.000000000000000000, 0.9510565162951535312, 1.000000000000000000, 0.9510565162951535312, 1.000000000000000000, 0.9510565162951535312, 1.000000000000000000, 0.9510565162951535312, 1.000000000000000000, 0.9510565162951535312, 1.000000000000000000, 0.9510565162951535312, 1.000000000000000000, 0.9510565162951535312, 1.000000000000000000, 0.9510565162951535312, 1.000000000000000000, 0.9510565162951535312, 1.000000000000000000, 0.9510565162951535312, 1.000000000000000000, 0.9510565162951535312, 1.000000000000000000, 0.9510565162951535312, 1.000000000000000000, 0.9510565162951535312, 1.000000000000000000, 0.9510565162951535312, 1.000000000000000000, 0.9510565162951535312, 1.000000000000000000, 0.9510565162951535312, 1.000000000000000000, 0.9510565162951535312, 1.000000000000000000, 0.9510565162951535312, 1.000000000000000000, 0.9510565162951535312, 1.000000000000000000, 0.9510565162951535312, 1.000000000000000000, 0.9510565162951535312, 1.000000000000000000, 0.9510565162951535312, 1.000000000000000000, 0.9510565162951535312, 1.000000000000000000, 0.9510565162951535312, 1.000000000000000000, 0.9510565162951535312, 1.000000000000000000, 0.9510565162951535312, 1.000000000000000000, 0.9510565162951535312, 1.000000000000000000, 0.9510565162951535312, 1.000000000000000000, 0.9510565162951535312, 1.000000000000000000, 0.9510565162951535312, 1.000000000000000000, 0.9510565162951535312, 1.000000000000000000, 0.9510565162951535312, 1.000000000000000000, 0.9510565162951535312, 1.000000000000000000, 0.9510565162951535312, 1.000000000000000000, 0.9510565162951535312, 1.000000000000000000, 0.9510565162951535312, 1.000000000000000000, 0.9510565162951535312, 1.000000000000000000, 0.9510565162951535312, 1.000000000000000000, 0.9510565162951535312, 1.000000000000000000, 0.9510565162951535312, 1.000000000000000000, 0.9510565162951535312, 1.000000000000000000, 0.9510565162951535312, 1.000000000000000000, 0.9510565162951535312, 1.000000000000000000, 0.9510565162951535312, 1.000000000000000000, 0.9510565162951535312, 1.000000000000000000, 0.9510565162951535312, 1.000000000000000000, 0.9510565162951535312, 1.000000000000000000, 0.9510565162951535312, 1.000000000000000000, 0.9510565162951535312, 1.000000000000000000, 0.9510565162951535312, 1.000000000000000000, 0.9510565162951535312, 1.000000000000000000, 0.9510565162951535312, 1.000000000000000000, 0.9510565162951535312, 1.000000000000000000, 0.9510565162951535312, 1.000000000000000000, 0.9510565162951535312, 1.000000000000000000, 0.9510565162951535312, 1.000000000000000000, 0.9510565162951535312, 1.000000000000000000, 0.9510565162951535312, 1.000000000000000000, 0.9510565162951535312, 1.000000000000000000, 0.9510565162951535312, 1.000000000000000000, 0.9510565162951535312, 1.000000000000000000, 0.9510565162951535312, 1.000000000000000000, 0.9510565162951535312, 1.000000000000000000, 0.9510565162951535312, 1.000000000000000000, 0.9510565162951535312, 1.000000000000000000, 0.9510565162951535312, 1.000000000000000000, 0.9510565162951535312, 1.000000000000000000, 0.9510565162951535312, 1.000000000000000000, 0.9510565162951535312, 1.000000000000000000, 0.9510565162951535312, 1.000000000000000000, 0.9510565162951535312, 1.000000000000000000, 0.9510565162951535312, 1.000000000000000000, 0.9510565162951535312, 1.000000000000000000, 0.9510565162951535312, 1.000000000000000000, 0.9510565162951535312, 1.000000000000000000, 0.9510565162951535312, 1.000000000000000000, 0.9510565162951535312, 1.000000000000000000, 0.9510565162951535312, 1.000000000000000000, 0.9510565162951535312, 1.000000000000000000, 0.9510565162951535312, 1.000000000000000000, 0.9510565162951535312, 1.000000000000000000, 0.9510565162951535312, 1.000000000000000000, 0.9510565162951535312, 1.000000000000000000, 0.9510565162951535312, 1.000000000000000000, 0.9510565162951535312, 1.000000000000000000, 0.9510565162951535312, 1.000000000000000000, 0.9510565162951535312, 1.000000000000000000, 0.9510565162951535312, 1.000000000000000000, 0.9510565162951535312, 1.000000000000000000, 0.9510565162951535312, 1.000000000000000000, 0.9510565162951535312, 1.000000000000000000, 0.9510565162951535312, 1.000000000000000000, 0.9510565162951535312, 1.000000000000000000, 0.9510565162951535312, 1.000000000000000000, 0.9510565162951535312, 1.000000000000000000, 0.9510565162951535312, 1.000000000000000000, 0.9510565162951535312, 1.000000000000000000, 0.9510565162951535312, 1.000000000000000000, 0.9510565162951535312, 1.000000000000000000, 0.9510565162951535312, 1.000000000000000000, 0.9510565162951535312, 1.000000000000000000, 0.9510565162951535312, 1.000000000000000000, 0.9510565162951535312, 1.000000000000000000, 0.9510565162951535312, 1.000000000000000000, 0.9510565162951535312, 1.000000000000000000, 0.9510565162951535312, 1.000000000000000000, 0.9510565162951535312, 1.000000000000000000, 0.9510565162951535312, 1.000000000000000000, 0.9510565162951535312, 1.000000000000000000, 0.9510565162951535312, 1.000000000000000000, 0.9510565162951535312, 1.000000000000000000, 0.9510565162951535312, 1.000000000000000000, 0.9510565162951535312, 1.000000000000000000, 0.9510565162951535312, 1.000000000000000000, 0.9510565162951535312, 1.000000000000000000, 0.9510565162951535312, 1.000000000000000000, 0.9510565162951535312, 1.000000000000000000, 0.9510565162951535312, 1.000000000000000000, 0.9510565162951535312, 1.000000000000000000, 0.9510565162951535312, 1.000000000000000000, 0.9510565162951535312, 1.000000000000000000, 0.9510565162951535312, 1.000000000000000000, 0.9510565162951535312, 1.000000000000000000, 0.9510565162951535312, 1.000000000000000000, 0.9510565162951535312, 1.000000000000000000, 0.9510565162951535312, 1.000000000000000000, 0.9510565162951535312, 1.000000000000000000, 0.9510565162951535312, 1.000000000000000000, 0.9510565162951535312, 1.000000000000000000, 0.9510565162951535312, 1.000000000000000000, 0.9510565162951535312, 1.000000000000000000, 0.9510565162951535312, 1.000000000000000000, 0.9510565162951535312, 1.000000000000000000, 0.9510565162951535312, 1.000000000000000000, 0.9510565162951535312, 1.000000000000000000, 0.9510565162951535312, 1.000000000000000000, 0.9510565162951535312, 1.000000000000000000, 0.9510565162951535312, 1.000000000000000000, 0.9510565162951535312, 1.000000000000000000, 0.9510565162951535312, 1.000000000000000000, 0.9510565162951535312, 1.000000000000000000, 0.9510565162951535312, 1.000000000000000000, 0.9510565162951535312, 1.000000000000000000, 0.9510565162951535312, 1.000000000000000000, 0.9510565162951535312, 1.000000000000000000, 0.9510565162951535312, 1.000000000000000000, 0.9510565162951535312, 1.000000000000000000, 0.9510565162951535312, 1.000000000000000000, 0.9836243115514193835, 0.9782066976764483002) ) ) 
 REPRESENTATION_ITEM ( '' )  SURFACE ( )  );
#6834 = CARTESIAN_POINT ( 'NONE',  ( -159.0959885057557983, -160.8584106276440480, 55.19815736654470584 ) ) ;
#6835 = CARTESIAN_POINT ( 'NONE',  ( -157.2955611005345986, -191.3438272943106995, 41.63779006702063867 ) ) ;
#6836 = CARTESIAN_POINT ( 'NONE',  ( 43.01140435219951286, 82.46049967264873715, 39.21067981925356349 ) ) ;
#6837 = DIRECTION ( 'NONE',  ( 0.000000000000000000, 0.000000000000000000, -1.000000000000000000 ) ) ;
#6838 = DIRECTION ( 'NONE',  ( 0.000000000000000000, 0.000000000000000000, 1.000000000000000000 ) ) ;
#6839 = CARTESIAN_POINT ( 'NONE',  ( 38.58424406990784661, 153.5297705074273154, 35.64915139335016647 ) ) ;
#6840 = LINE ( 'NONE', #1542, #10497 ) ;
#6841 = CARTESIAN_POINT ( 'NONE',  ( 75.16956835342354282, 131.6452004531123805, 5.196376467030073165 ) ) ;
#6842 = CARTESIAN_POINT ( 'NONE',  ( 47.43856463449117911, 145.4651871740939555, 35.64915139335015937 ) ) ;
#6843 = CARTESIAN_POINT ( 'NONE',  ( -148.5561028927606344, -164.7938272943107449, 40.69124936498395328 ) ) ;
#6844 = CARTESIAN_POINT ( 'NONE',  ( -151.4692556286852891, -173.9084106276440593, 39.74470866294723947 ) ) ;
#6845 = CARTESIAN_POINT ( 'NONE',  ( 43.01140435219951286, 70.46049967264873715, 39.21067981925356349 ) ) ;
#6846 = CARTESIAN_POINT ( 'NONE',  ( -148.5561028927606344, -159.0584106276440650, 40.69124936498395328 ) ) ;
#6847 = CARTESIAN_POINT ( 'NONE',  ( 28.99223550982291897, 144.4690685518502846, 2.342703524990218611 ) ) ;
#6848 = CARTESIAN_POINT ( 'NONE',  ( 54.85617982533816672, 239.2521282348021714, -19.99999999999996092 ) ) ;
#6849 = CARTESIAN_POINT ( 'NONE',  ( 38.58424406990784661, 120.2651871740939953, 35.64915139335016647 ) ) ;
#6850 = ORIENTED_EDGE ( 'NONE', *, *, #11475, .F. ) ;
#6851 = ORIENTED_EDGE ( 'NONE', *, *, #20870, .F. ) ;
#6852 = VERTEX_POINT ( 'NONE', #4673 ) ;
#6853 = CARTESIAN_POINT ( 'NONE',  ( 38.01140435219951996, 104.6344580088725564, 32.58608133808903773 ) ) ;
#6854 = CARTESIAN_POINT ( 'NONE',  ( 43.01140435219951286, 158.6297705074273381, 29.55568802177586107 ) ) ;
#6855 = CARTESIAN_POINT ( 'NONE',  ( 38.58424406990786082, 63.37977050742732388, 34.21067981925357060 ) ) ;
#6857 = CARTESIAN_POINT ( 'NONE',  ( 49.21618705061847265, 147.3337112213800140, -15.83906960951095577 ) ) ;
#6856 = CARTESIAN_POINT ( 'NONE',  ( 41.64333658814960870, 113.5151871740940095, 30.00020018409699318 ) ) ;
#6858 = VECTOR ( 'NONE', #18432, 1000.000000000000000 ) ;
#6859 = CARTESIAN_POINT ( 'NONE',  ( 38.01140435219951996, 84.86049967264872862, 35.83527830041810347 ) ) ;
#6860 = FACE_OUTER_BOUND ( 'NONE', #4280, .T. ) ;
#6861 = CARTESIAN_POINT ( 'NONE',  ( 43.80332655382220253, 98.88361825032845331, 29.21067981925356705 ) ) ;
#6862 = PLANE ( 'NONE',  #9020 ) ;
#6863 = AXIS2_PLACEMENT_3D ( 'NONE', #20277, #10572, #5280 ) ;
#6864 = CARTESIAN_POINT ( 'NONE',  ( 46.59305225739526435, 79.31518717409399244, 36.81289934271958941 ) ) ;
#6865 = CARTESIAN_POINT ( 'NONE',  ( 41.39828712335587113, 144.8568216812500680, 29.46674713776155130 ) ) ;
#6866 = CARTESIAN_POINT ( 'NONE',  ( 43.01140435219954838, 133.4604996726487514, 39.21067981925356349 ) ) ;
#6867 = ORIENTED_EDGE ( 'NONE', *, *, #6558, .F. ) ;
#6868 = CARTESIAN_POINT ( 'NONE',  ( 41.64333658814960870, 66.97977050742731819, 38.42115945441014446 ) ) ;
#6869 = CARTESIAN_POINT ( 'NONE',  ( -154.3824083646099439, -182.7584106276440536, 40.69124936498395328 ) ) ;
#6870 = CARTESIAN_POINT ( 'NONE',  ( 44.63232748576950115, 85.63068390643836381, -0.7129156696548789585 ) ) ;
#6871 = ADVANCED_FACE ( 'NONE', ( #16456, #3576 ), #15032, .T. ) ;
#6872 = CARTESIAN_POINT ( 'NONE',  ( -157.2955611005346270, -176.6084106276440195, 41.63779006702063867 ) ) ;
#6873 = EDGE_LOOP ( 'NONE', ( #14795, #16577, #123, #12391 ) ) ;
#6874 = CARTESIAN_POINT ( 'NONE',  ( 46.59305225739526435, 151.3151871740940067, 36.81289934271958941 ) ) ;
#6875 = CARTESIAN_POINT ( 'NONE',  ( 39.42975644700377558, 158.8151871740940067, 31.60846029578754468 ) ) ;
#6876 = CARTESIAN_POINT ( 'NONE',  ( 47.43856463449118621, 115.8797705074273097, 34.21067981925357060 ) ) ;
#6877 = CARTESIAN_POINT ( 'NONE',  ( 26.90790578767411390, 150.1165885900122987, 3.291480155758420345 ) ) ;
#6878 = ORIENTED_EDGE ( 'NONE', *, *, #21598, .F. ) ;
#6879 = SURFACE_STYLE_USAGE ( .BOTH. , #17993 ) ;
#6880 = EDGE_LOOP ( 'NONE', ( #20103, #284, #11378, #18183 ) ) ;
#6881 = CARTESIAN_POINT ( 'NONE',  ( 39.42975644700377558, 114.0797705074273125, 31.60846029578754468 ) ) ;
#6882 = CARTESIAN_POINT ( 'NONE',  ( 43.01140435219954838, 131.0344580088725479, 29.21067981925356705 ) ) ;
#6883 = CYLINDRICAL_SURFACE ( 'NONE', #18176, 21.90454335994848734 ) ;
#6884 = VECTOR ( 'NONE', #10224, 1000.000000000000227 ) ;
#6885 = CARTESIAN_POINT ( 'NONE',  ( 45.74753988029933538, 152.0651871740939782, 30.44471234641811819 ) ) ;
#6886 = CARTESIAN_POINT ( 'NONE',  ( 24.63684302007652249, 148.6959638282970957, 4.200683933265449532 ) ) ;
#6887 = SURFACE_SIDE_STYLE ('',( #6554 ) ) ;
#6888 = DIRECTION ( 'NONE',  ( 0.000000000000000000, 1.000000000000000000, 0.000000000000000000 ) ) ;
#6889 = CARTESIAN_POINT ( 'NONE',  ( -161.4692556286852607, -179.6391397928654783, 46.40781461928724383 ) ) ;
#6890 = CYLINDRICAL_SURFACE ( 'NONE', #8371, 10.00000000000000888 ) ;
#6891 = CARTESIAN_POINT ( 'NONE',  ( -153.0531000319306827, -195.1622583705451746, 39.65701158161629536 ) ) ;
#6892 = CARTESIAN_POINT ( 'NONE',  ( 48.01140435219951996, 97.43445800887256780, 32.58608133808903773 ) ) ;
#6893 = CARTESIAN_POINT ( 'NONE',  ( 38.96631938032478359, 98.48445800887257917, 31.27175355779120025 ) ) ;
#6894 = CARTESIAN_POINT ( 'NONE',  ( 38.58424406990784661, 93.22977050742730398, 32.77220824515698183 ) ) ;
#6895 =( BOUNDED_CURVE ( )  B_SPLINE_CURVE ( 2, ( #3634, #17274, #207, #10359, #3526, #1972, #16953, #2189, #8707, #14080, #18947, #20817, #11892 ),
 .UNSPECIFIED., .F., .F. ) 
 B_SPLINE_CURVE_WITH_KNOTS ( ( 3, 2, 2, 2, 2, 2, 3 ),
 ( 0.8897058823529412352, 0.8911764705882353477, 0.8941176470588235725, 0.8970588235294117974, 0.9000000000000000222, 0.9029411764705882470, 0.9044117647058823595 ),
 .UNSPECIFIED. ) 
 CURVE ( )  GEOMETRIC_REPRESENTATION_ITEM ( )  RATIONAL_B_SPLINE_CURVE ( ( 0.9755282581475768211, 0.9755282581475777093, 1.000000000000000000, 0.9510565162951535312, 1.000000000000000000, 0.9510565162951535312, 1.000000000000000000, 0.9510565162951535312, 1.000000000000000000, 0.9510565162951535312, 1.000000000000000000, 0.9755282581475768211, 0.9755282581475768211 ) ) 
 REPRESENTATION_ITEM ( '' )  );
#6896 = CARTESIAN_POINT ( 'NONE',  ( 43.64334309031418968, 148.0990856179656419, -3.057864931601543823 ) ) ;
#6897 = CARTESIAN_POINT ( 'NONE',  ( -157.2955611005346270, -170.3438272943107563, 41.63779006702063867 ) ) ;
#6898 = CARTESIAN_POINT ( 'NONE',  ( 46.59305225739526435, 79.31518717409399244, 36.81289934271958941 ) ) ;
#6899 = CARTESIAN_POINT ( 'NONE',  ( -154.5594255724347761, -169.8891397928654499, 59.16757674456785310 ) ) ;
#6900 = CYLINDRICAL_SURFACE ( 'NONE', #19935, 21.90454335994854063 ) ;
#6901 = AXIS2_PLACEMENT_3D ( 'NONE', #5052, #8480, #15188 ) ;
#6902 = ORIENTED_EDGE ( 'NONE', *, *, #17559, .F. ) ;
#6903 = CARTESIAN_POINT ( 'NONE',  ( -148.3790856849358306, -189.3891397928654783, 40.14644641866477315 ) ) ;
#6904 = DIRECTION ( 'NONE',  ( -0.3450121214752274179, 0.9385982292947088190, -7.395570986446985676E-32 ) ) ;
#6905 = CARTESIAN_POINT ( 'NONE',  ( 65.91867393726404600, 103.5983250578868109, 0.3515012976045437387 ) ) ;
#6906 = EDGE_CURVE ( 'NONE', #13154, #10374, #20438, .T. ) ;
#6907 = CARTESIAN_POINT ( 'NONE',  ( 173.3794444120442506, -84.13255853780189852, 5.000000000000018652 ) ) ;
#6908 = EDGE_LOOP ( 'NONE', ( #17800, #11088, #17201, #12718 ) ) ;
#6909 = CARTESIAN_POINT ( 'NONE',  ( 40.27526882409969033, 144.8297705074273267, 37.97664729208901946 ) ) ;
#6910 = CARTESIAN_POINT ( 'NONE',  ( 39.42975644700377558, 96.07977050742731251, 31.60846029578754468 ) ) ;
#6911 = CARTESIAN_POINT ( 'NONE',  ( 42.21948215057683740, 141.0373810949689926, 29.21067981925355994 ) ) ;
#6912 = CARTESIAN_POINT ( 'NONE',  ( 38.58424406990784661, 63.26518717409400239, 35.64915139335016647 ) ) ;
#6913 = DIRECTION ( 'NONE',  ( 1.000000000000000000, 0.000000000000000000, 0.000000000000000000 ) ) ;
#6914 = CARTESIAN_POINT ( 'NONE',  ( -155.3247640818417779, -155.4453048272798696, 40.99743929837026002 ) ) ;
#6915 = CARTESIAN_POINT ( 'NONE',  ( 43.01140435219951996, 10.71049967264875491, 29.21067981925357060 ) ) ;
#6916 = CARTESIAN_POINT ( 'NONE',  ( -141.4692556286852891, -165.2130981290893033, 52.90620854394536821 ) ) ;
#6917 = DIRECTION ( 'NONE',  ( 1.000000000000000000, 0.000000000000000000, 0.000000000000000000 ) ) ;
#6918 = FACE_OUTER_BOUND ( 'NONE', #4524, .T. ) ;
#6919 = EDGE_CURVE ( 'NONE', #3570, #5629, #11722, .T. ) ;
#6920 = CARTESIAN_POINT ( 'NONE',  ( 47.05648932407426344, 139.5844580088725877, 31.27175355779120025 ) ) ;
#6921 = CARTESIAN_POINT ( 'NONE',  ( 41.64333658814960870, 125.7797705074273296, 30.00020018409699318 ) ) ;
#6922 = CARTESIAN_POINT ( 'NONE',  ( 12.64719099284060988, 103.9244585094960769, 21.54915782717631600 ) ) ;
#6923 = CARTESIAN_POINT ( 'NONE',  ( 46.10157429594899270, 100.7344580088725792, 29.95742577749336988 ) ) ;
#6924 = CARTESIAN_POINT ( 'NONE',  ( 47.43856463449117911, 103.4651871740939839, 35.64915139335015937 ) ) ;
#6925 = DIRECTION ( 'NONE',  ( 0.000000000000000000, 0.000000000000000000, 1.000000000000000000 ) ) ;
#6926 = CARTESIAN_POINT ( 'NONE',  ( 37.47668497174467461, 153.6095807538456199, -2.346729193546184700 ) ) ;
#6927 = EDGE_CURVE ( 'NONE', #15878, #15277, #17005, .T. ) ;
#6928 = CARTESIAN_POINT ( 'NONE',  ( 18.86999673272213229, 105.3337293714367604, -5.438779171309367833 ) ) ;
#6929 = CARTESIAN_POINT ( 'NONE',  ( -176.9699209214867324, -136.9891397928655010, -72.64809332337415526 ) ) ;
#6930 = CARTESIAN_POINT ( 'NONE',  ( 45.74753988029934249, 88.42977050742729261, 37.97664729208901235 ) ) ;
#6931 = VECTOR ( 'NONE', #7320, 1000.000000000000000 ) ;
#6932 = VERTEX_POINT ( 'NONE', #1912 ) ;
#6933 = SHAPE_REPRESENTATION ( 'MAS-327', ( #8814, #19717, #2118, #5635, #7761, #17940, #14424, #1063, #11967, #18309, #9159, #16531, #15826, #5978, #8476 ), #8098 ) ;
#6934 = CARTESIAN_POINT ( 'NONE',  ( 48.01140435219951996, 134.3604996726487286, 32.58608133808903773 ) ) ;
#6935 = CARTESIAN_POINT ( 'NONE',  ( 38.01140435219951996, 68.93445800887255359, 35.83527830041810347 ) ) ;
#6936 = CARTESIAN_POINT ( 'NONE',  ( 41.46631938032478359, 87.38445800887258486, 38.96596240072933170 ) ) ;
#6937 = CARTESIAN_POINT ( 'NONE',  ( 44.55648932407425633, 133.6104996726487286, 38.96596240072933170 ) ) ;
#6939 = CARTESIAN_POINT ( 'NONE',  ( 68.96269327682742301, 142.1111764150114993, -15.20387477620461425 ) ) ;
#6938 = CARTESIAN_POINT ( 'NONE',  ( 45.74753988029933538, 92.06518717409399244, 30.44471234641811819 ) ) ;
#6940 = CIRCLE ( 'NONE', #19974, 24.99999999999998934 ) ;
#6941 = CARTESIAN_POINT ( 'NONE',  ( -157.2955611005346270, -157.7084106276440423, 57.67623309621198047 ) ) ;
#6942 = CARTESIAN_POINT ( 'NONE',  ( -160.8964159109769696, -185.0438272943107165, 46.59394152635518083 ) ) ;
#6943 = CARTESIAN_POINT ( 'NONE',  ( 38.01140435219952707, 93.56049967264874567, 32.58608133808903773 ) ) ;
#6944 = FACE_OUTER_BOUND ( 'NONE', #2598, .T. ) ;
#6945 = CYLINDRICAL_SURFACE ( 'NONE', #12111, 4.999999999999997335 ) ;
#6946 = CARTESIAN_POINT ( 'NONE',  ( -159.5594255724347761, -173.7891397928654840, 43.77915905869157598 ) ) ;
#6947 = CARTESIAN_POINT ( 'NONE',  ( 43.01140435219951286, 149.6297705074273097, 29.55568802177586463 ) ) ;
#6948 = CARTESIAN_POINT ( 'NONE',  ( 47.43856463449117200, 103.7297705074273182, 35.64915139335016647 ) ) ;
#6949 = CARTESIAN_POINT ( 'NONE',  ( 28.65042173108665935, 151.0721679115347911, -4.641026357035400451 ) ) ;
#6950 = CARTESIAN_POINT ( 'NONE',  ( 41.64333658814960870, 143.5151871740939953, 30.00020018409699318 ) ) ;
#6951 = CARTESIAN_POINT ( 'NONE',  ( 47.05648932407426344, 66.98445800887257917, 37.14960608071593384 ) ) ;
#6952 = CARTESIAN_POINT ( 'NONE',  ( -142.0420953463935803, -174.8084106276440082, 52.72008163687743831 ) ) ;
#6953 = CARTESIAN_POINT ( 'NONE',  ( 46.59305225739526435, 61.31518717409399954, 36.81289934271958941 ) ) ;
#6954 = CARTESIAN_POINT ( 'NONE',  ( -159.0959885057557983, -158.4584106276440423, 44.11586579668791330 ) ) ;
#6955 = CARTESIAN_POINT ( 'NONE',  ( 48.82767110959031243, 147.5835523268705458, -3.847861628839052361 ) ) ;
#6956 = FILL_AREA_STYLE ('',( #8394 ) ) ;
#6957 = CARTESIAN_POINT ( 'NONE',  ( 39.42975644700377558, 114.4151871740940010, 36.81289934271958941 ) ) ;
#6958 = AXIS2_PLACEMENT_3D ( 'NONE', #7777, #21221, #9647 ) ;
#6959 = EDGE_LOOP ( 'NONE', ( #2073, #2788, #11632, #5397 ) ) ;
#6960 = VERTEX_POINT ( 'NONE', #20226 ) ;
#6961 = CARTESIAN_POINT ( 'NONE',  ( 43.01140435219951286, 113.0344580088725763, 29.21067981925356705 ) ) ;
#6962 = ORIENTED_EDGE ( 'NONE', *, *, #15169, .F. ) ;
#6963 = ADVANCED_FACE ( 'NONE', ( #16899 ), #8648, .F. ) ;
#6964 = CARTESIAN_POINT ( 'NONE',  ( 47.05648932407426344, 100.5844580088725877, 31.27175355779120025 ) ) ;
#6965 = LINE ( 'NONE', #6754, #17803 ) ;
#6966 = CARTESIAN_POINT ( 'NONE',  ( 48.01140435219951996, 158.3604996726487286, 32.58608133808903773 ) ) ;
#6968 = CARTESIAN_POINT ( 'NONE',  ( 22.52008984372607614, 139.2495111981779985, 17.01435058386764965 ) ) ;
#6967 = CARTESIAN_POINT ( 'NONE',  ( 47.43856463449118621, 115.6151871740940038, 34.21067981925357060 ) ) ;
#6969 = CIRCLE ( 'NONE', #6239, 10.00000000000000888 ) ;
#6970 = CARTESIAN_POINT ( 'NONE',  ( 39.92123440845004723, 73.16049967264872578, 38.46393386101376421 ) ) ;
#6971 = CARTESIAN_POINT ( 'NONE',  ( 41.46631938032478359, 74.18445800887258201, 29.45539723777780239 ) ) ;
#6972 = EDGE_CURVE ( 'NONE', #4691, #137, #2061, .T. ) ;
#6973 = EDGE_CURVE ( 'NONE', #7422, #18986, #5277, .T. ) ;
#6974 = CARTESIAN_POINT ( 'NONE',  ( 38.01140435219952707, 71.78445800887257633, 34.21067981925357060 ) ) ;
#6975 = DIRECTION ( 'NONE',  ( -0.000000000000000000, -0.000000000000000000, -1.000000000000000000 ) ) ;
#6976 = CARTESIAN_POINT ( 'NONE',  ( 47.43856463449118621, 76.61518717409400381, 34.21067981925357060 ) ) ;
#6977 = CARTESIAN_POINT ( 'NONE',  ( 38.04401232081008288, 144.4086955619317507, 33.55330648861601617 ) ) ;
#6978 = VECTOR ( 'NONE', #9315, 1000.000000000000000 ) ;
#6979 = CARTESIAN_POINT ( 'NONE',  ( -148.5561028927606344, -176.7938272943107165, 40.69124936498395328 ) ) ;
#6980 = CARTESIAN_POINT ( 'NONE',  ( -151.4692556286852891, -196.9891397928655010, 49.65701158161630957 ) ) ;
#6981 = ORIENTED_EDGE ( 'NONE', *, *, #593, .T. ) ;
#6982 = CARTESIAN_POINT ( 'NONE',  ( -142.0420953463935803, -186.8084106276440650, 52.72008163687743831 ) ) ;
#6983 = CARTESIAN_POINT ( 'NONE',  ( 18.14018356548558941, 143.3940520581896862, 16.92415443696469879 ) ) ;
#6984 = CARTESIAN_POINT ( 'NONE',  ( -142.0420953463935803, -174.8084106276440082, 52.72008163687743831 ) ) ;
#6985 = ORIENTED_EDGE ( 'NONE', *, *, #868, .F. ) ;
#6986 = CARTESIAN_POINT ( 'NONE',  ( 38.58424406990786082, 156.1151871740940180, 34.21067981925357060 ) ) ;
#6987 = CARTESIAN_POINT ( 'NONE',  ( 41.64333658814960870, 158.5151871740940237, 30.00020018409699318 ) ) ;
#6988 = CARTESIAN_POINT ( 'NONE',  ( 44.37947211624943833, 116.4797705074273324, 30.00020018409699318 ) ) ;
#6989 = CARTESIAN_POINT ( 'NONE',  ( 13.78455932396994577, 137.7305411390292420, 2.696406107442721467 ) ) ;
#6990 = ORIENTED_EDGE ( 'NONE', *, *, #9487, .T. ) ;
#6991 = ORIENTED_EDGE ( 'NONE', *, *, #8037, .T. ) ;
#6992 = CARTESIAN_POINT ( 'NONE',  ( 44.37947211624943833, 109.2797705074273154, 38.42115945441014446 ) ) ;
#6993 = AXIS2_PLACEMENT_3D ( 'NONE', #21639, #4988, #19869 ) ;
#6994 = CARTESIAN_POINT ( 'NONE',  ( 43.01140435219951996, 158.0344580088725763, 29.21067981925357060 ) ) ;
#6995 = CARTESIAN_POINT ( 'NONE',  ( 43.01140435219951286, 127.4604996726487229, 39.21067981925356349 ) ) ;
#6996 = CARTESIAN_POINT ( 'NONE',  ( 40.27526882409969033, 144.5651871740939782, 37.97664729208901946 ) ) ;
#6997 = CARTESIAN_POINT ( 'NONE',  ( 43.80529445460960858, 154.1304981347762748, -3.137004163733609907 ) ) ;
#6998 = CARTESIAN_POINT ( 'NONE',  ( 43.80332655382220253, 82.95757658655229250, 29.21067981925356705 ) ) ;
#6999 = FACE_OUTER_BOUND ( 'NONE', #14526, .T. ) ;
#7000 = CARTESIAN_POINT ( 'NONE',  ( -161.4692556286852607, -173.3391397928654385, 52.90620854394536821 ) ) ;
#7001 = CARTESIAN_POINT ( 'NONE',  ( 48.01140435219951996, 101.0604996726487315, 35.83527830041809636 ) ) ;
#7002 = DIRECTION ( 'NONE',  ( 0.3428981916074309577, -0.9393725726208709270, 0.000000000000000000 ) ) ;
#7003 = CARTESIAN_POINT ( 'NONE',  ( 48.01140435219951996, 92.21049967264873715, 34.21067981925357060 ) ) ;
#7004 = CARTESIAN_POINT ( 'NONE',  ( 173.3794444120442506, -136.9891397928655010, 30.00000000000000000 ) ) ;
#7005 = CARTESIAN_POINT ( 'NONE',  ( 47.43856463449117200, 94.72977050742733240, 35.64915139335016647 ) ) ;
#7006 = CARTESIAN_POINT ( 'NONE',  ( 71.16904767199986281, 118.3707548728134213, -1.272037577920760665 ) ) ;
#7007 = CARTESIAN_POINT ( 'NONE',  ( -160.8964159109769696, -170.0438272943107449, 46.59394152635518793 ) ) ;
#7008 = CARTESIAN_POINT ( 'NONE',  ( 44.37947211624943833, 77.21518717409399812, 30.00020018409699318 ) ) ;
#7009 = DIRECTION ( 'NONE',  ( 0.000000000000000000, 1.000000000000000000, 0.000000000000000000 ) ) ;
#7010 = CARTESIAN_POINT ( 'NONE',  ( -161.4692556286853176, -158.4891397928654726, 49.65701158161630957 ) ) ;
#7011 = ORIENTED_EDGE ( 'NONE', *, *, #2754, .T. ) ;
#7012 = DIRECTION ( 'NONE',  ( 0.000000000000000000, 0.000000000000000000, 1.000000000000000000 ) ) ;
#7013 = CARTESIAN_POINT ( 'NONE',  ( 43.01140435219951996, 10.71049967264875491, 34.21067981925357060 ) ) ;
#7014 = CARTESIAN_POINT ( 'NONE',  ( 45.74753988029934249, 142.4297705074273210, 37.97664729208901235 ) ) ;
#7015 = CARTESIAN_POINT ( 'NONE',  ( 42.16380956469475194, 91.80013758078052888, 8.446644326836734606 ) ) ;
#7016 = ORIENTED_EDGE ( 'NONE', *, *, #18390, .T. ) ;
#7017 = CARTESIAN_POINT ( 'NONE',  ( -27.64582385433943656, -34.13255853780189142, 20.00000000000001776 ) ) ;
#7018 = VERTEX_POINT ( 'NONE', #11836 ) ;
#7019 = CARTESIAN_POINT ( 'NONE',  ( 41.64333658814960870, 134.7797705074273154, 30.00020018409699318 ) ) ;
#7020 = DIRECTION ( 'NONE',  ( 0.000000000000000000, 1.000000000000000000, 0.000000000000000000 ) ) ;
#7021 = AXIS2_PLACEMENT_3D ( 'NONE', #8149, #11327, #13209 ) ;
#7022 = CARTESIAN_POINT ( 'NONE',  ( 38.58424406990784661, 59.96518717409398391, 32.77220824515698183 ) ) ;
#7023 = DIRECTION ( 'NONE',  ( 0.000000000000000000, -1.000000000000000000, 0.000000000000000000 ) ) ;
#7024 =( BOUNDED_CURVE ( )  B_SPLINE_CURVE ( 2, ( #9203, #12933, #708, #16126, #4550, #921, #14145, #14247, #21210, #4229, #11270, #5769, #12820 ),
 .UNSPECIFIED., .F., .F. ) 
 B_SPLINE_CURVE_WITH_KNOTS ( ( 3, 2, 2, 2, 2, 2, 3 ),
 ( 0.5220588235294117974, 0.5235294117647059098, 0.5264705882352941346, 0.5294117647058823595, 0.5323529411764705843, 0.5352941176470588092, 0.5367647058823529216 ),
 .UNSPECIFIED. ) 
 CURVE ( )  GEOMETRIC_REPRESENTATION_ITEM ( )  RATIONAL_B_SPLINE_CURVE ( ( 0.9755282581475768211, 0.9755282581475768211, 1.000000000000000000, 0.9510565162951535312, 1.000000000000000000, 0.9510565162951535312, 1.000000000000000000, 0.9510565162951535312, 1.000000000000000000, 0.9510565162951535312, 1.000000000000000000, 0.9755282581475768211, 0.9755282581475768211 ) ) 
 REPRESENTATION_ITEM ( '' )  );
#7025 = DIRECTION ( 'NONE',  ( -0.000000000000000000, -0.000000000000000000, -1.000000000000000000 ) ) ;
#7026 = CARTESIAN_POINT ( 'NONE',  ( 43.01140435219951286, 107.9604996726487229, 29.21067981925356705 ) ) ;
#7027 = CARTESIAN_POINT ( 'NONE',  ( -143.3790856849358306, -167.7630981290893146, 43.77915905869157598 ) ) ;
#7028 = CARTESIAN_POINT ( 'NONE',  ( 41.46631938032478359, 143.1844580088725820, 29.45539723777780239 ) ) ;
#7029 = CARTESIAN_POINT ( 'NONE',  ( 45.74753988029933538, 124.4297705074273068, 37.97664729208901946 ) ) ;
#7030 = CARTESIAN_POINT ( 'NONE',  ( 18.91286941000743838, 105.1068529970173699, 0.5568269029779387980 ) ) ;
#7031 = FACE_OUTER_BOUND ( 'NONE', #4227, .T. ) ;
#7032 = CARTESIAN_POINT ( 'NONE',  ( 45.74753988029934249, 104.0651871740940067, 30.44471234641812174 ) ) ;
#7033 = DIRECTION ( 'NONE',  ( -0.000000000000000000, -0.000000000000000000, -1.000000000000000000 ) ) ;
#7034 = CARTESIAN_POINT ( 'NONE',  ( 60.49690154327523572, 149.3382625450468311, -9.565656633516235630 ) ) ;
#7035 = CARTESIAN_POINT ( 'NONE',  ( 15.38454125381035098, 114.2504036285165654, 1.942219256913226388 ) ) ;
#7036 = CARTESIAN_POINT ( 'NONE',  ( -141.4692556286852891, -156.2130981290893033, 52.90620854394536821 ) ) ;
#7037 =( GEOMETRIC_REPRESENTATION_CONTEXT ( 3 ) GLOBAL_UNCERTAINTY_ASSIGNED_CONTEXT ( ( #8652 ) ) GLOBAL_UNIT_ASSIGNED_CONTEXT ( ( #20926, #7378, #12539 ) ) REPRESENTATION_CONTEXT ( 'NONE', 'WORKASPACE' ) );
#7038 = CARTESIAN_POINT ( 'NONE',  ( 41.64333658814960870, 87.97977050742731819, 38.42115945441014446 ) ) ;
#7039 = EDGE_CURVE ( 'NONE', #6176, #2574, #8040, .T. ) ;
#7040 = VERTEX_POINT ( 'NONE', #15256 ) ;
#7041 = CARTESIAN_POINT ( 'NONE',  ( 38.96631938032478359, 75.08445800887257349, 37.14960608071593384 ) ) ;
#7042 = LINE ( 'NONE', #18718, #330 ) ;
#7043 = CARTESIAN_POINT ( 'NONE',  ( 48.01140435219951996, 128.0604996726487457, 35.83527830041810347 ) ) ;
#7045 = CARTESIAN_POINT ( 'NONE',  ( 32.54106024366770811, 152.4163610972421452, -16.51355214031335805 ) ) ;
#7044 = CARTESIAN_POINT ( 'NONE',  ( 43.01140435219951286, 86.36518717409400381, 29.55568802177586463 ) ) ;
#7046 = CARTESIAN_POINT ( 'NONE',  ( -155.3247660971248933, -155.7098880568450738, 40.99743995317544432 ) ) ;
#7047 = CARTESIAN_POINT ( 'NONE',  ( -151.4692556286852891, -176.6438272943107108, 39.74470866294723947 ) ) ;
#7048 = DIRECTION ( 'NONE',  ( 0.000000000000000000, 0.000000000000000000, 1.000000000000000000 ) ) ;
#7049 = CARTESIAN_POINT ( 'NONE',  ( -161.4692556286852607, -193.4130981290893203, 52.90620854394536821 ) ) ;
#7050 = DIRECTION ( 'NONE',  ( 0.000000000000000000, 0.000000000000000000, 1.000000000000000000 ) ) ;
#7051 = APPLICATION_CONTEXT ( 'automotive_design' ) ;
#7052 = CARTESIAN_POINT ( 'NONE',  ( 38.01140435219952707, 92.63445800887258486, 32.58608133808903773 ) ) ;
#7053 = CARTESIAN_POINT ( 'NONE',  ( 48.01140435219951996, 143.2104996726487514, 34.21067981925357060 ) ) ;
#7054 = CARTESIAN_POINT ( 'NONE',  ( 47.43856463449118621, 154.8797705074273097, 34.21067981925357060 ) ) ;
#7055 = CARTESIAN_POINT ( 'NONE',  ( 41.64333658814960870, 102.9797705074273182, 38.42115945441014446 ) ) ;
#7056 = CARTESIAN_POINT ( 'NONE',  ( 53.70366401737062034, 152.5123965792994625, -3.808113302951443568 ) ) ;
#7057 = CARTESIAN_POINT ( 'NONE',  ( 38.58424406990785371, 138.2651871740939669, 35.64915139335015937 ) ) ;
#7058 = FACE_BOUND ( 'NONE', #16559, .T. ) ;
#7059 = CARTESIAN_POINT ( 'NONE',  ( -154.3824083646099439, -169.5584106276440366, 58.62277379824867296 ) ) ;
#7060 = CARTESIAN_POINT ( 'NONE',  ( 43.80332655382220253, 90.61133943119284595, 39.21067981925355639 ) ) ;
#7061 = CARTESIAN_POINT ( 'NONE',  ( 17.08493018425929932, 131.2036312357472241, 1.628145005703640624 ) ) ;
#7062 =( NAMED_UNIT ( * ) SI_UNIT ( $, .STERADIAN. ) SOLID_ANGLE_UNIT ( ) );
#7063 = CARTESIAN_POINT ( 'NONE',  ( 40.27526882409969033, 119.6651871740939868, 30.44471234641811819 ) ) ;
#7064 = ORIENTED_EDGE ( 'NONE', *, *, #20142, .F. ) ;
#7065 = ORIENTED_EDGE ( 'NONE', *, *, #4231, .F. ) ;
#7066 = VECTOR ( 'NONE', #441, 1000.000000000000000 ) ;
#7067 = AXIS2_PLACEMENT_3D ( 'NONE', #18803, #6267, #18054 ) ;
#7068 = CARTESIAN_POINT ( 'NONE',  ( -153.0531000319306827, -180.1622583705451746, 39.65701158161629536 ) ) ;
#7069 = EDGE_LOOP ( 'NONE', ( #21676, #4181, #2335, #8722 ) ) ;
#7070 = CARTESIAN_POINT ( 'NONE',  ( 47.05648932407426344, 103.5844580088725877, 31.27175355779120025 ) ) ;
#7071 = CARTESIAN_POINT ( 'NONE',  ( 38.58424406990785371, 156.5297705074273154, 35.64915139335015937 ) ) ;
#7072 = EDGE_CURVE ( 'NONE', #12353, #16672, #4898, .T. ) ;
#7073 = CARTESIAN_POINT ( 'NONE',  ( 44.37947211624943833, 61.27977050742732246, 38.42115945441014446 ) ) ;
#7075 = CARTESIAN_POINT ( 'NONE',  ( 58.12682455153977656, 96.19528378222683784, -13.22021563155647428 ) ) ;
#7074 = CARTESIAN_POINT ( 'NONE',  ( 39.42975644700377558, 117.4151871740940010, 36.81289934271958941 ) ) ;
#7076 = ADVANCED_FACE ( 'NONE', ( #14914 ), #11944, .T. ) ;
#7077 = CARTESIAN_POINT ( 'NONE',  ( 41.46631938032478359, 73.31049967264874567, 38.96596240072933170 ) ) ;
#7079 = CARTESIAN_POINT ( 'NONE',  ( 43.01140435219951286, 137.0344580088725763, 29.21067981925356705 ) ) ;
#7078 = CARTESIAN_POINT ( 'NONE',  ( 24.43941541943582862, 313.3049502139530205, 272.0939500981630204 ) ) ;
#7080 = CARTESIAN_POINT ( 'NONE',  ( 43.01140435219951286, 122.9604996726487371, 29.21067981925356705 ) ) ;
#7081 = CARTESIAN_POINT ( 'NONE',  ( 46.06263289999436239, 95.09248412622439162, 30.23627618186981536 ) ) ;
#7082 = CARTESIAN_POINT ( 'NONE',  ( 43.01140435219951286, 104.9604996726487371, 29.21067981925356705 ) ) ;
#7083 = CARTESIAN_POINT ( 'NONE',  ( -154.3824083646099439, -179.4938272943107336, 40.69124936498395328 ) ) ;
#7084 = CARTESIAN_POINT ( 'NONE',  ( 162.3411339277076308, 184.7625696037766261, 272.0939500981630204 ) ) ;
#7085 = EDGE_LOOP ( 'NONE', ( #1463, #8666, #18935, #12489 ) ) ;
#7086 = CARTESIAN_POINT ( 'NONE',  ( -142.0420953463935803, -189.5084106276440536, 46.59394152635518793 ) ) ;
#7087 = CARTESIAN_POINT ( 'NONE',  ( 53.04203944364535772, 87.17698241397053494, 14.00585298808814194 ) ) ;
#7088 = CARTESIAN_POINT ( 'NONE',  ( -154.3824083646099439, -175.5584106276440366, 58.62277379824867296 ) ) ;
#7089 = ORIENTED_EDGE ( 'NONE', *, *, #19577, .F. ) ;
#7090 = CARTESIAN_POINT ( 'NONE',  ( 47.43856463449117200, 139.4651871740940123, 35.64915139335016647 ) ) ;
#7091 = CARTESIAN_POINT ( 'NONE',  ( -143.9637021292202235, -116.9891397928655010, 36.65701158161628825 ) ) ;
#7092 = CARTESIAN_POINT ( 'NONE',  ( 46.59305225739526435, 101.1797705074273210, 31.60846029578754468 ) ) ;
#7093 = CARTESIAN_POINT ( 'NONE',  ( 8.798315742295939046, 121.0924013121165075, 9.124689178586496752 ) ) ;
#7094 = ORIENTED_EDGE ( 'NONE', *, *, #5263, .T. ) ;
#7095 = EDGE_CURVE ( 'NONE', #5296, #1608, #21772, .T. ) ;
#7096 = CARTESIAN_POINT ( 'NONE',  ( 71.19791805076843616, 120.7596060772701776, 5.632536115698772328 ) ) ;
#7097 = ORIENTED_EDGE ( 'NONE', *, *, #20930, .T. ) ;
#7098 = CARTESIAN_POINT ( 'NONE',  ( 44.37947211624943833, 113.4797705074273324, 30.00020018409699318 ) ) ;
#7099 = CARTESIAN_POINT ( 'NONE',  ( 39.92123440845005433, 158.3344580088725877, 29.95742577749336988 ) ) ;
#7100 = DIRECTION ( 'NONE',  ( 0.9385982292947088190, 0.3450121214752276955, -0.000000000000000000 ) ) ;
#7101 = CARTESIAN_POINT ( 'NONE',  ( 43.01140435219951286, 141.8651871740940180, 38.86567161673127657 ) ) ;
#7102 = MANIFOLD_SOLID_BREP ( 'Chamfer1', #13383 ) ;
#7103 = CARTESIAN_POINT ( 'NONE',  ( 47.05648932407426344, 97.91049967264873999, 37.14960608071593384 ) ) ;
#7104 = CARTESIAN_POINT ( 'NONE',  ( 17.60877916486148465, 96.95950790538488206, 1.267834678905774393 ) ) ;
#7105 = CARTESIAN_POINT ( 'NONE',  ( -143.3790856849358306, -179.7630981290893146, 43.77915905869157598 ) ) ;
#7106 = CARTESIAN_POINT ( 'NONE',  ( -148.3790856849358306, -174.3891397928654783, 40.14644641866477315 ) ) ;
#7107 = CARTESIAN_POINT ( 'NONE',  ( -104.7439762501682736, 39.86119447055682485, -19.99999999999997868 ) ) ;
#7108 = CARTESIAN_POINT ( 'NONE',  ( 147.5268905834513475, 193.0332408774651185, 14.00000000000001776 ) ) ;
#7109 = PLANE ( 'NONE',  #7667 ) ;
#7110 = CARTESIAN_POINT ( 'NONE',  ( 41.64333658814960870, 80.77977050742732956, 30.00020018409699318 ) ) ;
#7111 = CARTESIAN_POINT ( 'NONE',  ( 44.18632541912793243, 91.73153706005567187, -6.629209314582290347 ) ) ;
#7112 = CARTESIAN_POINT ( 'NONE',  ( -154.3824083646099439, -176.4938272943107336, 40.69124936498395328 ) ) ;
#7113 = CARTESIAN_POINT ( 'NONE',  ( 41.64333658814960870, 74.51518717409399528, 30.00020018409699318 ) ) ;
#7114 = CARTESIAN_POINT ( 'NONE',  ( -153.0531000319306827, -171.1622583705452030, 39.65701158161629536 ) ) ;
#7115 = FACE_OUTER_BOUND ( 'NONE', #3781, .T. ) ;
#7116 = VERTEX_POINT ( 'NONE', #4084 ) ;
#7117 = CARTESIAN_POINT ( 'NONE',  ( 41.46631938032478359, 118.3104996726487457, 38.96596240072933170 ) ) ;
#7118 = CARTESIAN_POINT ( 'NONE',  ( 48.01140435219951996, 122.2104996726487371, 34.21067981925357060 ) ) ;
#7119 = CARTESIAN_POINT ( 'NONE',  ( 40.27526882409969744, 134.9297705074272642, 30.44471234641812174 ) ) ;
#7120 = CARTESIAN_POINT ( 'NONE',  ( 69.71546013739904879, 111.0973159356150717, 7.018072855358342466 ) ) ;
#7121 = ORIENTED_EDGE ( 'NONE', *, *, #20373, .F. ) ;
#7122 = DIRECTION ( 'NONE',  ( -0.000000000000000000, -0.000000000000000000, 1.000000000000000000 ) ) ;
#7123 = ORIENTED_EDGE ( 'NONE', *, *, #21327, .F. ) ;
#7124 = CARTESIAN_POINT ( 'NONE',  ( 41.64333658814960870, 140.7797705074273154, 30.00020018409699318 ) ) ;
#7125 = VECTOR ( 'NONE', #11815, 1000.000000000000000 ) ;
#7126 = CIRCLE ( 'NONE', #15222, 10.00000000000000888 ) ;
#7127 = CARTESIAN_POINT ( 'NONE',  ( 45.74753988029933538, 92.32977050742731251, 30.44471234641811819 ) ) ;
#7128 = AXIS2_PLACEMENT_3D ( 'NONE', #11236, #18488, #19507 ) ;
#7129 = CARTESIAN_POINT ( 'NONE',  ( 43.01140435219951996, 119.9070776186055838, -35.00000000000000000 ) ) ;
#7130 = CARTESIAN_POINT ( 'NONE',  ( -27.64582385433943656, -34.13255853780189142, 5.000000000000018652 ) ) ;
#7131 = LINE ( 'NONE', #5887, #684 ) ;
#7132 = CARTESIAN_POINT ( 'NONE',  ( 38.58424406990784661, 101.9651871740939981, 32.77220824515698183 ) ) ;
#7133 = CARTESIAN_POINT ( 'NONE',  ( 38.96631938032478359, 153.4104996726487400, 31.27175355779120025 ) ) ;
#7134 = DIRECTION ( 'NONE',  ( -0.5061580162706792452, -0.8624407588727069918, 0.000000000000000000 ) ) ;
#7135 = CARTESIAN_POINT ( 'NONE',  ( -157.6495955161842062, -173.0130981290893146, 41.15050349809590102 ) ) ;
#7136 = DIRECTION ( 'NONE',  ( 1.000000000000000000, 0.000000000000000000, 0.000000000000000000 ) ) ;
#7137 = CARTESIAN_POINT ( 'NONE',  ( 39.92123440845004723, 147.2344580088725650, 38.46393386101376421 ) ) ;
#7138 = CARTESIAN_POINT ( 'NONE',  ( 41.64333658814960870, 114.9797705074273324, 38.42115945441014446 ) ) ;
#7139 = CARTESIAN_POINT ( 'NONE',  ( 9.157865646370469292, 114.3054763464604662, 21.90616645148510599 ) ) ;
#7140 = CARTESIAN_POINT ( 'NONE',  ( 43.80332655382220253, 100.9575765865522925, 29.21067981925356705 ) ) ;
#7141 = MANIFOLD_SOLID_BREP ( 'Cut-Extrude13', #16898 ) ;
#7142 = CARTESIAN_POINT ( 'NONE',  ( 41.64333658814960870, 102.7151871740939981, 38.42115945441014446 ) ) ;
#7143 = VERTEX_POINT ( 'NONE', #21664 ) ;
#7144 = DIRECTION ( 'NONE',  ( 0.000000000000000000, 0.000000000000000000, 1.000000000000000000 ) ) ;
#7145 = CARTESIAN_POINT ( 'NONE',  ( 20.91437931538276374, 145.9617080342048894, -10.94665030085253044 ) ) ;
#7146 = CARTESIAN_POINT ( 'NONE',  ( 42.95897134029118547, 91.70801217734280897, 7.418363685804686192 ) ) ;
#7147 = DIRECTION ( 'NONE',  ( 0.000000000000000000, 0.000000000000000000, 1.000000000000000000 ) ) ;
#7148 = CARTESIAN_POINT ( 'NONE',  ( 41.64333658814960870, 90.97977050742731819, 38.42115945441014446 ) ) ;
#7149 = ORIENTED_EDGE ( 'NONE', *, *, #19173, .T. ) ;
#7150 =( BOUNDED_CURVE ( )  B_SPLINE_CURVE ( 2, ( #12014, #10165, #18313, #4864, #11802, #6854, #15110, #16758, #20403, #341, #20091, #5302, #16865, #5194, #16649, #18748, #3213, #3651, #11912, #7071, #10379, #8616, #1780, #8514, #15226, #3324, #1560, #19979, #18641, #4980, #11691, #17079, #20195, #1670, #1992, #125, #8289, #11584, #13561, #10269, #14, #8724, #8402, #15442, #14994, #21737, #12559, #17186, #19177, #18851, #19286, #8835, #13881, #2308, #7177, #17510, #9047, #10698, #14099, #12233, #3759, #2419, #7292, #20727, #4185, #17619, #20834, #18964, #2524, #5726, #769, #12449, #4076, #10486, #20620, #10807, #5504, #9158, #7505, #3866, #2206, #8938, #15644, #548, #13991, #5613, #12338, #2706, #1387, #1059, #9881, #19797, #18249, #8229, #8116, #21239, #18019, #17905, #12961, #16365, #8011, #21565, #6456, #19911, #10099, #16807, #5243, #11738, #8455, #18691, #281, #15160, #12064, #7014, #1931, #1722, #1828, #13718, #3489, #8336, #20454, #172, #5135, #2043, #20031, #15048, #14931, #21679, #13293, #4916, #11629, #16697, #21787, #6694, #13401, #60, #13510, #20243, #18582, #10213, #12609, #7442, #19331, #2464, #4124, #20993, #5770, #10534, #709, #2148, #10746, #2359, #8774, #12499, #20774, #4230, #10958, #17667, #493, #10859, #19226, #814, #5665, #7119, #15489, #15694, #17450, #3914, #20669, #9204, #391, #17232, #17557, #599, #9098, #20565, #15903, #13826, #7551, #15799, #5448, #7340, #14039, #14248, #5878, #12167, #5550, #12389, #18900, #2252, #19124, #3807, #8881, #14146, #13930, #15588, #20882, #7230, #4018, #12277, #19013, #10641, #17344, #8987, #4551, #4770, #16447, #7771, #4331, #7984, #12714, #16127, #16010, #14469, #7666, #14689, #11056, #13152, #2905, #21539, #14798, #9310, #11382, #4436, #9533, #6430, #11166, #21429, #2677, #16230, #11491, #6093, #17879, #6319, #21211, #2792, #13045, #9750, #1142, #19882, #1360, #9419, #16340, #12822, #2571, #14363, #9640, #19540, #11271, #14576, #17990, #21105, #1034, #1248, #19769, #4666, #922, #18105, #5987, #19438, #17771, #7876, #3012, #21318, #8091, #6204, #19658, #6542, #16888, #250, #11932, #13583, #8637, #15247, #20001, #10186, #11606, #20215, #1902, #15359, #21759, #5108, #145, #1471, #13267, #1802, #6988, #18663, #20320, #13692, #6876, #4885, #5219, #18334, #11824, #18557, #18218, #3567, #3235, #9967, #20426, #10291, #5322, #3124, #9854, #21653, #16556, #8203, #14904, #16670, #1582, #8310, #10073, #15019, #6667, #13374, #20111, #5002, #11712, #18447, #3345, #16782, #1693, #8424, #15133, #35, #6776, #13483, #3462, #15665, #681, #5524, #18984, #12469, #19199, #12359, #17204, #4096, #19097, #14117, #568, #15776, #7418, #20855, #5637, #5745, #14013, #14225, #10831, #2120, #13797, #17422, #365, #3779, #3670, #8856, #17100, #2329, #20535, #790, #3995, #17529, #10400, #18769, #2438, #13902, #3888, #15876, #20641, #9068, #12138, #10611, #20965, #15563, #12253, #9179, #466, #17317, #7524, #12038, #2227, #8958, #2016, #18872, #10719, #7199, #8747, #15464, #7092, #7312, #20746, #5421, #10508, #10932, #5961, #13203, #1524, #8254, #16721, #8143, #3288, #11548, #17639, #2546, #6483, #1008, #14848, #18157, #21593, #9284, #12687, #19939, #14955, #21702, #1632, #4825, #10017, #15984, #7634, #11653, #18389, #3064, #18276, #3178, #895, #21078, #9907, #8364, #6602, #13320, #15075, #16613, #19408, #20057, #4307, #4943, #5850, #12581, #19306, #11031, #17746, #4203, #2649, #9391, #16097, #7744, #14445, #21180, #6070, #12797, #19516, #4410, #11431, #9804, #16498, #1415, #7148, #3403, #5373, #20164, #13852, #309, #8910, #20588, #20372, #13635, #5473, #18934, #8801, #11877, #3621, #10455, #15300, #6930, #416, #12197, #7038, #5158, #3834, #13744, #2072, #15412, #10562, #10127, #8691, #21812, #18819, #20483, #11984, #6720, #18608, #10236, #17261, #16937, #8481, #5053, #12089, #18714, #15514, #2174, #3725, #13426, #11765, #17156, #92, #10343, #18496, #16833, #3513, #1852, #6824, #1746, #17046, #15189, #13531, #8583, #20266, #193, #5269, #1958, #5797, #12745, #950, #2597, #12419, #2494, #9336, #521, #740, #9236, #10775, #5696, #16037, #17799, #2277, #17695, #7472, #15934, #5580, #7695, #20696, #10669, #15727, #4156, #9015, #19359, #19256, #12529, #10886, #14068, #13958, #2710, #845, #12305, #4047, #12637, #14281, #19043, #7580, #14392, #11085, #17588, #21026, #19466, #3941, #5909, #15613, #4256, #10984, #21131, #7257, #19147, #17482, #6014, #2391, #630, #17372, #4356, #7366, #20804, #9127, #15827, #14177, #20912, #6458, #9557, #6346, #20033, #7795, #12964, #4578, #16263, #13180, #21456, #3152, #11522, #11298, #9884, #17908, #21682, #9453, #2931, #6577, #16583, #18252, #6232, #18130, #1502, #19800, #2819, #8120, #16367, #18024, #19569, #1278, #21344, #8232, #19913, #4799, #8014, #21242, #13297, #12849, #11195, #14933, #4918, #19686, #7902, #9778, #11631, #18360, #16153, #1064, #6120, #11406, #1169, #14605, #9667, #14500, #4464, #14720, #3039, #13072, #4690, #16473, #1389, #14822, #21568, #18473, #17132, #15276, #1606, #18797, #11741, #15492, #3265, #174, #5350, #18585, #16700, #10102, #11963, #3700, #13612, #3377, #1935, #10215, #20246, #13405 ),
 .UNSPECIFIED., .F., .T. ) 
 B_SPLINE_CURVE_WITH_KNOTS ( ( 3, 2, 2, 2, 2, 2, 2, 2, 2, 2, 2, 2, 2, 2, 2, 2, 2, 2, 2, 2, 2, 2, 2, 2, 2, 2, 2, 2, 2, 2, 2, 2, 2, 2, 2, 2, 2, 2, 2, 2, 2, 2, 2, 2, 2, 2, 2, 2, 2, 2, 2, 2, 2, 2, 2, 2, 2, 2, 2, 2, 2, 2, 2, 2, 2, 2, 2, 2, 2, 2, 2, 2, 2, 2, 2, 2, 2, 2, 2, 2, 2, 2, 2, 2, 2, 2, 2, 2, 2, 2, 2, 2, 2, 2, 2, 2, 2, 2, 2, 2, 2, 2, 2, 2, 2, 2, 2, 2, 2, 2, 2, 2, 2, 2, 2, 2, 2, 2, 2, 2, 2, 2, 2, 2, 2, 2, 2, 2, 2, 2, 2, 2, 2, 2, 2, 2, 2, 2, 2, 2, 2, 2, 2, 2, 2, 2, 2, 2, 2, 2, 2, 2, 2, 2, 2, 2, 2, 2, 2, 2, 2, 2, 2, 2, 2, 2, 2, 2, 2, 2, 2, 2, 2, 2, 2, 2, 2, 2, 2, 2, 2, 2, 2, 2, 2, 2, 2, 2, 2, 2, 2, 2, 2, 2, 2, 2, 2, 2, 2, 2, 2, 2, 2, 2, 2, 2, 2, 2, 2, 2, 2, 2, 2, 2, 2, 2, 2, 2, 2, 2, 2, 2, 2, 2, 2, 2, 2, 2, 2, 2, 2, 2, 2, 2, 2, 2, 2, 2, 2, 2, 2, 2, 2, 2, 2, 2, 2, 2, 2, 2, 2, 2, 2, 2, 2, 2, 2, 2, 2, 2, 2, 2, 2, 2, 2, 2, 2, 2, 2, 2, 2, 2, 2, 2, 2, 2, 2, 2, 2, 2, 2, 2, 2, 2, 2, 2, 2, 2, 2, 2, 2, 2, 2, 2, 2, 2, 2, 2, 2, 2, 2, 2, 2, 2, 2, 2, 2, 2, 2, 2, 2, 2, 2, 2, 2, 2, 2, 2, 2, 2, 2, 2, 2, 2, 2, 2, 2, 2, 2, 2, 2, 2, 2, 2, 3 ),
 ( 0.000000000000000000, 0.002941176470588235253, 0.005882352941176470507, 0.008823529411764705760, 0.01176470588235294101, 0.01470588235294117627, 0.01764705882352941152, 0.02058823529411764677, 0.02352941176470588203, 0.02647058823529411728, 0.02941176470588235253, 0.03235294117647059126, 0.03529411764705882304, 0.03823529411764706176, 0.04117647058823529355, 0.04411764705882353227, 0.04705882352941176405, 0.05000000000000000278, 0.05294117647058823456, 0.05588235294117647328, 0.05882352941176470507, 0.06176470588235294379, 0.06470588235294118251, 0.06764705882352940736, 0.07058823529411764608, 0.07352941176470588480, 0.07647058823529412352, 0.07941176470588234837, 0.08235294117647058709, 0.08529411764705882582, 0.08823529411764706454, 0.09117647058823530326, 0.09411764705882352811, 0.09705882352941176683, 0.1000000000000000056, 0.1029411764705882304, 0.1058823529411764691, 0.1088235294117647078, 0.1117647058823529466, 0.1147058823529411714, 0.1176470588235294101, 0.1205882352941176489, 0.1235294117647058876, 0.1264705882352941124, 0.1294117647058823650, 0.1323529411764705899, 0.1352941176470588147, 0.1382352941176470673, 0.1411764705882352922, 0.1441176470588235170, 0.1470588235294117696, 0.1499999999999999944, 0.1529411764705882470, 0.1558823529411764719, 0.1588235294117646967, 0.1617647058823529493, 0.1647058823529411742, 0.1676470588235293990, 0.1705882352941176516, 0.1735294117647058765, 0.1764705882352941291, 0.1794117647058823539, 0.1823529411764706065, 0.1852941176470588314, 0.1882352941176470562, 0.1911764705882352811, 0.1941176470588235337, 0.1970588235294117585, 0.2000000000000000111, 0.2029411764705882359, 0.2058823529411764608, 0.2088235294117647134, 0.2117647058823529382, 0.2147058823529411631, 0.2176470588235294157, 0.2205882352941176405, 0.2235294117647058931, 0.2264705882352941180, 0.2294117647058823428, 0.2323529411764705954, 0.2352941176470588203, 0.2382352941176470451, 0.2411764705882352977, 0.2441176470588235226, 0.2470588235294117752, 0.2500000000000000000, 0.2529411764705882248, 0.2558823529411764497, 0.2588235294117647300, 0.2617647058823529549, 0.2647058823529411797, 0.2676470588235294046, 0.2705882352941176294, 0.2735294117647059098, 0.2764705882352941346, 0.2794117647058823595, 0.2823529411764705843, 0.2852941176470588092, 0.2882352941176470340, 0.2911764705882353144, 0.2941176470588235392, 0.2970588235294117641, 0.2999999999999999889, 0.3029411764705882137, 0.3058823529411764941, 0.3088235294117647189, 0.3117647058823529438, 0.3147058823529411686, 0.3176470588235293935, 0.3205882352941176738, 0.3235294117647058987, 0.3264705882352941235, 0.3294117647058823484, 0.3323529411764705732, 0.3352941176470587981, 0.3382352941176470784, 0.3411764705882353033, 0.3441176470588235281, 0.3470588235294117530, 0.3499999999999999778, 0.3529411764705882582, 0.3558823529411764830, 0.3588235294117647078, 0.3617647058823529327, 0.3647058823529412130, 0.3676470588235294379, 0.3705882352941176627, 0.3735294117647058876, 0.3764705882352941124, 0.3794117647058823373, 0.3823529411764705621, 0.3852941176470587870, 0.3882352941176470673, 0.3911764705882352922, 0.3941176470588235170, 0.3970588235294117418, 0.4000000000000000222, 0.4029411764705882470, 0.4058823529411764719, 0.4088235294117646967, 0.4117647058823529216, 0.4147058823529412019, 0.4176470588235294268, 0.4205882352941176516, 0.4235294117647058765, 0.4264705882352941013, 0.4294117647058823262, 0.4323529411764706065, 0.4352941176470588314, 0.4382352941176470562, 0.4411764705882352811, 0.4441176470588235059, 0.4470588235294117863, 0.4500000000000000111, 0.4529411764705882359, 0.4558823529411764608, 0.4588235294117646856, 0.4617647058823529660, 0.4647058823529411908, 0.4676470588235294157, 0.4705882352941176405, 0.4735294117647058654, 0.4764705882352940902, 0.4794117647058823706, 0.4823529411764705954, 0.4852941176470588203, 0.4882352941176470451, 0.4911764705882352700, 0.4941176470588235503, 0.4970588235294117752, 0.5000000000000000000, 0.5029411764705882248, 0.5058823529411764497, 0.5088235294117646745, 0.5117647058823528994, 0.5147058823529411242, 0.5176470588235294601, 0.5205882352941176849, 0.5235294117647059098, 0.5264705882352941346, 0.5294117647058823595, 0.5323529411764705843, 0.5352941176470588092, 0.5382352941176470340, 0.5411764705882352589, 0.5441176470588234837, 0.5470588235294118196, 0.5500000000000000444, 0.5529411764705882693, 0.5558823529411764941, 0.5588235294117647189, 0.5617647058823529438, 0.5647058823529411686, 0.5676470588235293935, 0.5705882352941176183, 0.5735294117647058432, 0.5764705882352940680, 0.5794117647058824039, 0.5823529411764706287, 0.5852941176470588536, 0.5882352941176470784, 0.5911764705882353033, 0.5941176470588235281, 0.5970588235294117530, 0.5999999999999999778, 0.6029411764705882026, 0.6058823529411764275, 0.6088235294117646523, 0.6117647058823529882, 0.6147058823529412130, 0.6176470588235294379, 0.6205882352941176627, 0.6235294117647058876, 0.6264705882352941124, 0.6294117647058823373, 0.6323529411764705621, 0.6352941176470587870, 0.6382352941176470118, 0.6411764705882353477, 0.6441176470588235725, 0.6470588235294117974, 0.6500000000000000222, 0.6529411764705882470, 0.6558823529411764719, 0.6588235294117646967, 0.6617647058823529216, 0.6647058823529411464, 0.6676470588235293713, 0.6705882352941175961, 0.6735294117647059320, 0.6764705882352941568, 0.6794117647058823817, 0.6823529411764706065, 0.6852941176470588314, 0.6882352941176470562, 0.6911764705882352811, 0.6941176470588235059, 0.6970588235294117307, 0.6999999999999999556, 0.7029411764705881804, 0.7058823529411765163, 0.7088235294117647411, 0.7117647058823529660, 0.7147058823529411908, 0.7176470588235294157, 0.7205882352941176405, 0.7235294117647058654, 0.7264705882352940902, 0.7294117647058824261, 0.7323529411764705399, 0.7352941176470588758, 0.7382352941176471006, 0.7411764705882353255, 0.7441176470588235503, 0.7470588235294117752, 0.7499999999999998890, 0.7529411764705882248, 0.7558823529411764497, 0.7588235294117646745, 0.7617647058823528994, 0.7647058823529411242, 0.7676470588235294601, 0.7705882352941175739, 0.7735294117647059098, 0.7764705882352941346, 0.7794117647058823595, 0.7823529411764705843, 0.7852941176470588092, 0.7882352941176470340, 0.7911764705882352589, 0.7941176470588234837, 0.7970588235294118196, 0.8000000000000000444, 0.8029411764705882693, 0.8058823529411764941, 0.8088235294117647189, 0.8117647058823529438, 0.8147058823529411686, 0.8176470588235293935, 0.8205882352941176183, 0.8235294117647058432, 0.8264705882352940680, 0.8294117647058824039, 0.8323529411764706287, 0.8352941176470588536, 0.8382352941176470784, 0.8411764705882353033, 0.8441176470588235281, 0.8470588235294117530, 0.8499999999999999778, 0.8529411764705882026, 0.8558823529411764275, 0.8588235294117646523, 0.8617647058823529882, 0.8647058823529412130, 0.8676470588235294379, 0.8705882352941176627, 0.8735294117647058876, 0.8764705882352941124, 0.8794117647058823373, 0.8823529411764705621, 0.8852941176470587870, 0.8882352941176470118, 0.8911764705882353477, 0.8941176470588235725, 0.8970588235294117974, 0.9000000000000000222, 0.9029411764705882470, 0.9058823529411764719, 0.9088235294117646967, 0.9117647058823529216, 0.9147058823529411464, 0.9176470588235293713, 0.9205882352941175961, 0.9235294117647059320, 0.9264705882352941568, 0.9294117647058823817, 0.9323529411764706065, 0.9352941176470588314, 0.9382352941176470562, 0.9411764705882352811, 0.9441176470588235059, 0.9470588235294117307, 0.9499999999999999556, 0.9529411764705881804, 0.9558823529411765163, 0.9588235294117647411, 0.9617647058823529660, 0.9647058823529411908, 0.9676470588235294157, 0.9705882352941176405, 0.9735294117647058654, 0.9764705882352940902, 0.9794117647058823151, 0.9803958342062288889 ),
 .UNSPECIFIED. ) 
 CURVE ( )  GEOMETRIC_REPRESENTATION_ITEM ( )  RATIONAL_B_SPLINE_CURVE ( ( 1.000000000000000000, 0.9510565162951535312, 1.000000000000000000, 0.9510565162951535312, 1.000000000000000000, 0.9510565162951535312, 1.000000000000000000, 0.9510565162951535312, 1.000000000000000000, 0.9510565162951535312, 1.000000000000000000, 0.9510565162951535312, 1.000000000000000000, 0.9510565162951535312, 1.000000000000000000, 0.9510565162951535312, 1.000000000000000000, 0.9510565162951535312, 1.000000000000000000, 0.9510565162951535312, 1.000000000000000000, 0.9510565162951535312, 1.000000000000000000, 0.9510565162951535312, 1.000000000000000000, 0.9510565162951535312, 1.000000000000000000, 0.9510565162951535312, 1.000000000000000000, 0.9510565162951535312, 1.000000000000000000, 0.9510565162951535312, 1.000000000000000000, 0.9510565162951535312, 1.000000000000000000, 0.9510565162951535312, 1.000000000000000000, 0.9510565162951535312, 1.000000000000000000, 0.9510565162951535312, 1.000000000000000000, 0.9510565162951535312, 1.000000000000000000, 0.9510565162951535312, 1.000000000000000000, 0.9510565162951535312, 1.000000000000000000, 0.9510565162951535312, 1.000000000000000000, 0.9510565162951535312, 1.000000000000000000, 0.9510565162951535312, 1.000000000000000000, 0.9510565162951535312, 1.000000000000000000, 0.9510565162951535312, 1.000000000000000000, 0.9510565162951535312, 1.000000000000000000, 0.9510565162951535312, 1.000000000000000000, 0.9510565162951535312, 1.000000000000000000, 0.9510565162951535312, 1.000000000000000000, 0.9510565162951535312, 1.000000000000000000, 0.9510565162951535312, 1.000000000000000000, 0.9510565162951535312, 1.000000000000000000, 0.9510565162951535312, 1.000000000000000000, 0.9510565162951535312, 1.000000000000000000, 0.9510565162951535312, 1.000000000000000000, 0.9510565162951535312, 1.000000000000000000, 0.9510565162951535312, 1.000000000000000000, 0.9510565162951535312, 1.000000000000000000, 0.9510565162951535312, 1.000000000000000000, 0.9510565162951535312, 1.000000000000000000, 0.9510565162951535312, 1.000000000000000000, 0.9510565162951535312, 1.000000000000000000, 0.9510565162951535312, 1.000000000000000000, 0.9510565162951535312, 1.000000000000000000, 0.9510565162951535312, 1.000000000000000000, 0.9510565162951535312, 1.000000000000000000, 0.9510565162951535312, 1.000000000000000000, 0.9510565162951535312, 1.000000000000000000, 0.9510565162951535312, 1.000000000000000000, 0.9510565162951535312, 1.000000000000000000, 0.9510565162951535312, 1.000000000000000000, 0.9510565162951535312, 1.000000000000000000, 0.9510565162951535312, 1.000000000000000000, 0.9510565162951535312, 1.000000000000000000, 0.9510565162951535312, 1.000000000000000000, 0.9510565162951535312, 1.000000000000000000, 0.9510565162951535312, 1.000000000000000000, 0.9510565162951535312, 1.000000000000000000, 0.9510565162951535312, 1.000000000000000000, 0.9510565162951535312, 1.000000000000000000, 0.9510565162951535312, 1.000000000000000000, 0.9510565162951535312, 1.000000000000000000, 0.9510565162951535312, 1.000000000000000000, 0.9510565162951535312, 1.000000000000000000, 0.9510565162951535312, 1.000000000000000000, 0.9510565162951535312, 1.000000000000000000, 0.9510565162951535312, 1.000000000000000000, 0.9510565162951535312, 1.000000000000000000, 0.9510565162951535312, 1.000000000000000000, 0.9510565162951535312, 1.000000000000000000, 0.9510565162951535312, 1.000000000000000000, 0.9510565162951535312, 1.000000000000000000, 0.9510565162951535312, 1.000000000000000000, 0.9510565162951535312, 1.000000000000000000, 0.9510565162951535312, 1.000000000000000000, 0.9510565162951535312, 1.000000000000000000, 0.9510565162951535312, 1.000000000000000000, 0.9510565162951535312, 1.000000000000000000, 0.9510565162951535312, 1.000000000000000000, 0.9510565162951535312, 1.000000000000000000, 0.9510565162951535312, 1.000000000000000000, 0.9510565162951535312, 1.000000000000000000, 0.9510565162951535312, 1.000000000000000000, 0.9510565162951535312, 1.000000000000000000, 0.9510565162951535312, 1.000000000000000000, 0.9510565162951535312, 1.000000000000000000, 0.9510565162951535312, 1.000000000000000000, 0.9510565162951535312, 1.000000000000000000, 0.9510565162951535312, 1.000000000000000000, 0.9510565162951535312, 1.000000000000000000, 0.9510565162951535312, 1.000000000000000000, 0.9510565162951535312, 1.000000000000000000, 0.9510565162951535312, 1.000000000000000000, 0.9510565162951535312, 1.000000000000000000, 0.9510565162951535312, 1.000000000000000000, 0.9510565162951535312, 1.000000000000000000, 0.9510565162951535312, 1.000000000000000000, 0.9510565162951535312, 1.000000000000000000, 0.9510565162951535312, 1.000000000000000000, 0.9510565162951535312, 1.000000000000000000, 0.9510565162951535312, 1.000000000000000000, 0.9510565162951535312, 1.000000000000000000, 0.9510565162951535312, 1.000000000000000000, 0.9510565162951535312, 1.000000000000000000, 0.9510565162951535312, 1.000000000000000000, 0.9510565162951535312, 1.000000000000000000, 0.9510565162951535312, 1.000000000000000000, 0.9510565162951535312, 1.000000000000000000, 0.9510565162951535312, 1.000000000000000000, 0.9510565162951535312, 1.000000000000000000, 0.9510565162951535312, 1.000000000000000000, 0.9510565162951535312, 1.000000000000000000, 0.9510565162951535312, 1.000000000000000000, 0.9510565162951535312, 1.000000000000000000, 0.9510565162951535312, 1.000000000000000000, 0.9510565162951535312, 1.000000000000000000, 0.9510565162951535312, 1.000000000000000000, 0.9510565162951535312, 1.000000000000000000, 0.9510565162951535312, 1.000000000000000000, 0.9510565162951535312, 1.000000000000000000, 0.9510565162951535312, 1.000000000000000000, 0.9510565162951535312, 1.000000000000000000, 0.9510565162951535312, 1.000000000000000000, 0.9510565162951535312, 1.000000000000000000, 0.9510565162951535312, 1.000000000000000000, 0.9510565162951535312, 1.000000000000000000, 0.9510565162951535312, 1.000000000000000000, 0.9510565162951535312, 1.000000000000000000, 0.9510565162951535312, 1.000000000000000000, 0.9510565162951535312, 1.000000000000000000, 0.9510565162951535312, 1.000000000000000000, 0.9510565162951535312, 1.000000000000000000, 0.9510565162951535312, 1.000000000000000000, 0.9510565162951535312, 1.000000000000000000, 0.9510565162951535312, 1.000000000000000000, 0.9510565162951535312, 1.000000000000000000, 0.9510565162951535312, 1.000000000000000000, 0.9510565162951535312, 1.000000000000000000, 0.9510565162951535312, 1.000000000000000000, 0.9510565162951535312, 1.000000000000000000, 0.9510565162951535312, 1.000000000000000000, 0.9510565162951535312, 1.000000000000000000, 0.9510565162951535312, 1.000000000000000000, 0.9510565162951535312, 1.000000000000000000, 0.9510565162951535312, 1.000000000000000000, 0.9510565162951535312, 1.000000000000000000, 0.9510565162951535312, 1.000000000000000000, 0.9510565162951535312, 1.000000000000000000, 0.9510565162951535312, 1.000000000000000000, 0.9510565162951535312, 1.000000000000000000, 0.9510565162951535312, 1.000000000000000000, 0.9510565162951535312, 1.000000000000000000, 0.9510565162951535312, 1.000000000000000000, 0.9510565162951535312, 1.000000000000000000, 0.9510565162951535312, 1.000000000000000000, 0.9510565162951535312, 1.000000000000000000, 0.9510565162951535312, 1.000000000000000000, 0.9510565162951535312, 1.000000000000000000, 0.9510565162951535312, 1.000000000000000000, 0.9510565162951535312, 1.000000000000000000, 0.9510565162951535312, 1.000000000000000000, 0.9510565162951535312, 1.000000000000000000, 0.9510565162951535312, 1.000000000000000000, 0.9510565162951535312, 1.000000000000000000, 0.9510565162951535312, 1.000000000000000000, 0.9510565162951535312, 1.000000000000000000, 0.9510565162951535312, 1.000000000000000000, 0.9510565162951535312, 1.000000000000000000, 0.9510565162951535312, 1.000000000000000000, 0.9510565162951535312, 1.000000000000000000, 0.9510565162951535312, 1.000000000000000000, 0.9510565162951535312, 1.000000000000000000, 0.9510565162951535312, 1.000000000000000000, 0.9510565162951535312, 1.000000000000000000, 0.9510565162951535312, 1.000000000000000000, 0.9510565162951535312, 1.000000000000000000, 0.9510565162951535312, 1.000000000000000000, 0.9510565162951535312, 1.000000000000000000, 0.9510565162951535312, 1.000000000000000000, 0.9510565162951535312, 1.000000000000000000, 0.9510565162951535312, 1.000000000000000000, 0.9510565162951535312, 1.000000000000000000, 0.9510565162951535312, 1.000000000000000000, 0.9510565162951535312, 1.000000000000000000, 0.9510565162951535312, 1.000000000000000000, 0.9510565162951535312, 1.000000000000000000, 0.9510565162951535312, 1.000000000000000000, 0.9510565162951535312, 1.000000000000000000, 0.9510565162951535312, 1.000000000000000000, 0.9510565162951535312, 1.000000000000000000, 0.9510565162951535312, 1.000000000000000000, 0.9510565162951535312, 1.000000000000000000, 0.9510565162951535312, 1.000000000000000000, 0.9510565162951535312, 1.000000000000000000, 0.9510565162951535312, 1.000000000000000000, 0.9510565162951535312, 1.000000000000000000, 0.9510565162951535312, 1.000000000000000000, 0.9510565162951535312, 1.000000000000000000, 0.9510565162951535312, 1.000000000000000000, 0.9510565162951535312, 1.000000000000000000, 0.9510565162951535312, 1.000000000000000000, 0.9510565162951535312, 1.000000000000000000, 0.9510565162951535312, 1.000000000000000000, 0.9510565162951535312, 1.000000000000000000, 0.9510565162951535312, 1.000000000000000000, 0.9510565162951535312, 1.000000000000000000, 0.9510565162951535312, 1.000000000000000000, 0.9510565162951535312, 1.000000000000000000, 0.9510565162951535312, 1.000000000000000000, 0.9510565162951535312, 1.000000000000000000, 0.9510565162951535312, 1.000000000000000000, 0.9510565162951535312, 1.000000000000000000, 0.9510565162951535312, 1.000000000000000000, 0.9510565162951535312, 1.000000000000000000, 0.9510565162951535312, 1.000000000000000000, 0.9510565162951535312, 1.000000000000000000, 0.9510565162951535312, 1.000000000000000000, 0.9510565162951535312, 1.000000000000000000, 0.9510565162951535312, 1.000000000000000000, 0.9510565162951535312, 1.000000000000000000, 0.9510565162951535312, 1.000000000000000000, 0.9510565162951535312, 1.000000000000000000, 0.9510565162951535312, 1.000000000000000000, 0.9510565162951535312, 1.000000000000000000, 0.9510565162951535312, 1.000000000000000000, 0.9510565162951535312, 1.000000000000000000, 0.9510565162951535312, 1.000000000000000000, 0.9510565162951535312, 1.000000000000000000, 0.9510565162951535312, 1.000000000000000000, 0.9510565162951535312, 1.000000000000000000, 0.9510565162951535312, 1.000000000000000000, 0.9510565162951535312, 1.000000000000000000, 0.9510565162951535312, 1.000000000000000000, 0.9510565162951535312, 1.000000000000000000, 0.9510565162951535312, 1.000000000000000000, 0.9510565162951535312, 1.000000000000000000, 0.9510565162951535312, 1.000000000000000000, 0.9510565162951535312, 1.000000000000000000, 0.9510565162951535312, 1.000000000000000000, 0.9510565162951535312, 1.000000000000000000, 0.9510565162951535312, 1.000000000000000000, 0.9510565162951535312, 1.000000000000000000, 0.9510565162951535312, 1.000000000000000000, 0.9510565162951535312, 1.000000000000000000, 0.9510565162951535312, 1.000000000000000000, 0.9510565162951535312, 1.000000000000000000, 0.9510565162951535312, 1.000000000000000000, 0.9510565162951535312, 1.000000000000000000, 0.9510565162951535312, 1.000000000000000000, 0.9510565162951535312, 1.000000000000000000, 0.9510565162951535312, 1.000000000000000000, 0.9510565162951535312, 1.000000000000000000, 0.9510565162951535312, 1.000000000000000000, 0.9510565162951535312, 1.000000000000000000, 0.9510565162951535312, 1.000000000000000000, 0.9510565162951535312, 1.000000000000000000, 0.9510565162951535312, 1.000000000000000000, 0.9510565162951535312, 1.000000000000000000, 0.9510565162951535312, 1.000000000000000000, 0.9510565162951535312, 1.000000000000000000, 0.9510565162951535312, 1.000000000000000000, 0.9510565162951535312, 1.000000000000000000, 0.9510565162951535312, 1.000000000000000000, 0.9510565162951535312, 1.000000000000000000, 0.9510565162951535312, 1.000000000000000000, 0.9510565162951535312, 1.000000000000000000, 0.9510565162951535312, 1.000000000000000000, 0.9510565162951535312, 1.000000000000000000, 0.9510565162951535312, 1.000000000000000000, 0.9510565162951535312, 1.000000000000000000, 0.9510565162951535312, 1.000000000000000000, 0.9510565162951535312, 1.000000000000000000, 0.9510565162951535312, 1.000000000000000000, 0.9510565162951535312, 1.000000000000000000, 0.9510565162951535312, 1.000000000000000000, 0.9510565162951535312, 1.000000000000000000, 0.9510565162951535312, 1.000000000000000000, 0.9510565162951535312, 1.000000000000000000, 0.9510565162951535312, 1.000000000000000000, 0.9510565162951535312, 1.000000000000000000, 0.9510565162951535312, 1.000000000000000000, 0.9510565162951535312, 1.000000000000000000, 0.9510565162951535312, 1.000000000000000000, 0.9510565162951535312, 1.000000000000000000, 0.9510565162951535312, 1.000000000000000000, 0.9510565162951535312, 1.000000000000000000, 0.9510565162951535312, 1.000000000000000000, 0.9510565162951535312, 1.000000000000000000, 0.9510565162951535312, 1.000000000000000000, 0.9510565162951535312, 1.000000000000000000, 0.9510565162951535312, 1.000000000000000000, 0.9510565162951535312, 1.000000000000000000, 0.9510565162951535312, 1.000000000000000000, 0.9510565162951535312, 1.000000000000000000, 0.9510565162951535312, 1.000000000000000000, 0.9510565162951535312, 1.000000000000000000, 0.9510565162951535312, 1.000000000000000000, 0.9510565162951535312, 1.000000000000000000, 0.9510565162951535312, 1.000000000000000000, 0.9510565162951535312, 1.000000000000000000, 0.9510565162951535312, 1.000000000000000000, 0.9510565162951535312, 1.000000000000000000, 0.9510565162951535312, 1.000000000000000000, 0.9510565162951535312, 1.000000000000000000, 0.9510565162951535312, 1.000000000000000000, 0.9510565162951535312, 1.000000000000000000, 0.9510565162951535312, 1.000000000000000000, 0.9510565162951535312, 1.000000000000000000, 0.9510565162951535312, 1.000000000000000000, 0.9510565162951535312, 1.000000000000000000, 0.9510565162951535312, 1.000000000000000000, 0.9510565162951535312, 1.000000000000000000, 0.9510565162951535312, 1.000000000000000000, 0.9510565162951535312, 1.000000000000000000, 0.9510565162951535312, 1.000000000000000000, 0.9510565162951535312, 1.000000000000000000, 0.9510565162951535312, 1.000000000000000000, 0.9510565162951535312, 1.000000000000000000, 0.9510565162951535312, 1.000000000000000000, 0.9510565162951535312, 1.000000000000000000, 0.9510565162951535312, 1.000000000000000000, 0.9510565162951535312, 1.000000000000000000, 0.9510565162951535312, 1.000000000000000000, 0.9510565162951535312, 1.000000000000000000, 0.9510565162951535312, 1.000000000000000000, 0.9510565162951535312, 1.000000000000000000, 0.9510565162951535312, 1.000000000000000000, 0.9510565162951535312, 1.000000000000000000, 0.9510565162951535312, 1.000000000000000000, 0.9510565162951535312, 1.000000000000000000, 0.9836243115514193835, 0.9782066976764483002 ) ) 
 REPRESENTATION_ITEM ( '' )  );
#7151 = CARTESIAN_POINT ( 'NONE',  ( 43.01140435219951286, 75.53445800887256212, 39.46799094044489209 ) ) ;
#7152 = CARTESIAN_POINT ( 'NONE',  ( -143.3790856849358306, -172.2891397928654840, 55.53486410454105027 ) ) ;
#7153 = CARTESIAN_POINT ( 'NONE',  ( 38.01140435219951996, 129.8604996726487286, 35.83527830041810347 ) ) ;
#7155 = CARTESIAN_POINT ( 'NONE',  ( 32.43765954726634959, 145.6647664193251615, 11.44158087452429129 ) ) ;
#7154 = CARTESIAN_POINT ( 'NONE',  ( 41.64333658814960870, 86.51518717409399528, 30.00020018409699318 ) ) ;
#7156 = CARTESIAN_POINT ( 'NONE',  ( -151.4692556286852891, -157.4084106276440593, 59.56931450028537967 ) ) ;
#7157 = CARTESIAN_POINT ( 'NONE',  ( -154.3824083646099439, -178.2938272943107165, 58.62277379824867296 ) ) ;
#7158 = CARTESIAN_POINT ( 'NONE',  ( 39.92123440845005433, 117.2344580088725792, 38.46393386101375711 ) ) ;
#7159 = DIRECTION ( 'NONE',  ( 0.000000000000000000, 1.000000000000000000, 0.000000000000000000 ) ) ;
#7160 = CARTESIAN_POINT ( 'NONE',  ( 41.46631938032478359, 81.38445800887257064, 38.96596240072933170 ) ) ;
#7161 = CARTESIAN_POINT ( 'NONE',  ( -151.4692556286852891, -196.9891397928655010, 39.65701158161630246 ) ) ;
#7162 = CARTESIAN_POINT ( 'NONE',  ( 147.5268905834513475, 193.0332408774651185, 14.00000000000001776 ) ) ;
#7163 = CARTESIAN_POINT ( 'NONE',  ( 45.74753988029933538, 152.3297705074272699, 30.44471234641811819 ) ) ;
#7164 = CARTESIAN_POINT ( 'NONE',  ( 38.58424406990784661, 105.2297705074273040, 32.77220824515698183 ) ) ;
#7165 = CARTESIAN_POINT ( 'NONE',  ( 71.08298874133512868, 139.6419663798271529, -3.093729572736475752 ) ) ;
#7166 = CARTESIAN_POINT ( 'NONE',  ( 38.58424406990785371, 134.9651871740940123, 32.77220824515697473 ) ) ;
#7167 = FACE_OUTER_BOUND ( 'NONE', #19414, .T. ) ;
#7168 = CARTESIAN_POINT ( 'NONE',  ( -148.5561028927606344, -169.2584106276440536, 58.62277379824867296 ) ) ;
#7169 = DIRECTION ( 'NONE',  ( -0.9385982292947088190, -0.3450121214752274179, 2.040824802394967185E-16 ) ) ;
#7170 = CARTESIAN_POINT ( 'NONE',  ( 37.76446383830448639, 92.11682557054228937, 6.628417810721723313 ) ) ;
#7171 = CARTESIAN_POINT ( 'NONE',  ( 148.6725454929228079, -61.68114226949890622, 30.00000000000000000 ) ) ;
#7172 = CARTESIAN_POINT ( 'NONE',  ( 38.58424406990784661, 111.2651871740939811, 35.64915139335016647 ) ) ;
#7173 = ORIENTED_EDGE ( 'NONE', *, *, #7768, .F. ) ;
#7174 = CARTESIAN_POINT ( 'NONE',  ( -158.9748091281504401, -116.9891397928655010, 36.65701158161628115 ) ) ;
#7175 = VERTEX_POINT ( 'NONE', #10814 ) ;
#7176 = CARTESIAN_POINT ( 'NONE',  ( 44.55648932407425633, 103.8844580088725849, 29.45539723777780239 ) ) ;
#7177 = CARTESIAN_POINT ( 'NONE',  ( 44.37947211624943833, 151.2797705074273438, 38.42115945441014446 ) ) ;
#7178 = CARTESIAN_POINT ( 'NONE',  ( 38.96631938032478359, 154.0104996726487343, 37.14960608071593384 ) ) ;
#7180 = CARTESIAN_POINT ( 'NONE',  ( 70.04389262751028866, 127.6510855156269599, -14.64878692017946626 ) ) ;
#7179 = CARTESIAN_POINT ( 'NONE',  ( 45.74753988029933538, 115.1651871740940010, 37.97664729208901946 ) ) ;
#7182 = CARTESIAN_POINT ( 'NONE',  ( 47.05648932407426344, 68.51049967264874851, 31.27175355779120025 ) ) ;
#7181 = PRODUCT_RELATED_PRODUCT_CATEGORY ( 'part', '', ( #21567 ) ) ;
#7184 = CARTESIAN_POINT ( 'NONE',  ( 42.21948215057684450, 75.45757658655230671, 39.21067981925355639 ) ) ;
#7183 = CARTESIAN_POINT ( 'NONE',  ( 45.65510909715900567, 144.7672780766941401, 29.96360841760569116 ) ) ;
#7185 = CARTESIAN_POINT ( 'NONE',  ( 41.46631938032478359, 123.1104996726487570, 29.45539723777780239 ) ) ;
#7186 = CARTESIAN_POINT ( 'NONE',  ( 47.25797261159726759, 95.27021368899106335, 31.56623162037505637 ) ) ;
#7187 = CARTESIAN_POINT ( 'NONE',  ( 39.42975644700377558, 77.81518717409399244, 31.60846029578754468 ) ) ;
#7188 = CARTESIAN_POINT ( 'NONE',  ( 137.5268905834513191, 193.0332408774651185, -50.99999999999998579 ) ) ;
#7189 = CARTESIAN_POINT ( 'NONE',  ( -160.8964159109769696, -184.7438272943107052, 52.72008163687743121 ) ) ;
#7190 = CARTESIAN_POINT ( 'NONE',  ( -142.0420953463935803, -192.8084106276440366, 52.72008163687743831 ) ) ;
#7191 = EDGE_CURVE ( 'NONE', #15486, #21451, #6055, .T. ) ;
#7192 = EDGE_LOOP ( 'NONE', ( #247, #6095, #16178, #3883 ) ) ;
#7193 = CARTESIAN_POINT ( 'NONE',  ( -151.4692556286852891, -181.4084106276440025, 59.56931450028537967 ) ) ;
#7194 = CARTESIAN_POINT ( 'NONE',  ( 75.59501567365037999, 109.4093883240155378, 12.93430809701916750 ) ) ;
#7195 = ORIENTED_EDGE ( 'NONE', *, *, #18362, .T. ) ;
#7196 = CARTESIAN_POINT ( 'NONE',  ( 39.42975644700377558, 143.8151871740940067, 31.60846029578754468 ) ) ;
#7197 = FACE_OUTER_BOUND ( 'NONE', #742, .T. ) ;
#7198 = ADVANCED_FACE ( 'NONE', ( #2750 ), #11019, .T. ) ;
#7199 = CARTESIAN_POINT ( 'NONE',  ( 43.01140435219951286, 101.6297705074273239, 29.55568802177586107 ) ) ;
#7200 = CARTESIAN_POINT ( 'NONE',  ( 76.79083979644461522, 114.3551126354810492, -1.232281421064668869 ) ) ;
#7201 = VERTEX_POINT ( 'NONE', #19186 ) ;
#7202 = CARTESIAN_POINT ( 'NONE',  ( 68.03731475862628031, 132.9047928164914367, -1.867435455408581912 ) ) ;
#7203 = ORIENTED_EDGE ( 'NONE', *, *, #3264, .T. ) ;
#7204 = AXIS2_PLACEMENT_3D ( 'NONE', #15996, #11152, #16432 ) ;
#7205 = EDGE_CURVE ( 'NONE', #16099, #17658, #17369, .T. ) ;
#7206 = PLANE ( 'NONE',  #14231 ) ;
#7207 = CARTESIAN_POINT ( 'NONE',  ( 43.80332655382220253, 88.53738109496899256, 39.21067981925355639 ) ) ;
#7208 = CARTESIAN_POINT ( 'NONE',  ( 43.01140435219951286, 83.62977050742730967, 29.55568802177586463 ) ) ;
#7209 = CARTESIAN_POINT ( 'NONE',  ( 41.64333658814960870, 140.5151871740939953, 30.00020018409699318 ) ) ;
#7210 = AXIS2_PLACEMENT_3D ( 'NONE', #13862, #2082, #11995 ) ;
#7211 = MANIFOLD_SOLID_BREP ( 'Thread2', #4950 ) ;
#7212 = CARTESIAN_POINT ( 'NONE',  ( 46.10157429594899270, 103.7604996726487627, 38.46393386101376421 ) ) ;
#7213 = CARTESIAN_POINT ( 'NONE',  ( 11.67247064774405452, 106.1322524520788875, 1.624861436118421043 ) ) ;
#7214 = CARTESIAN_POINT ( 'NONE',  ( 44.55648932407425633, 118.6104996726487570, 38.96596240072933170 ) ) ;
#7215 = CARTESIAN_POINT ( 'NONE',  ( -143.3790856849358306, -165.6891397928654897, 43.77915905869157598 ) ) ;
#7216 = DIRECTION ( 'NONE',  ( 0.000000000000000000, 0.000000000000000000, 1.000000000000000000 ) ) ;
#7217 = CYLINDRICAL_SURFACE ( 'NONE', #20627, 14.42424326798555434 ) ;
#7218 = CARTESIAN_POINT ( 'NONE',  ( 43.80332655382220253, 151.9575765865523067, 29.21067981925356705 ) ) ;
#7219 = CARTESIAN_POINT ( 'NONE',  ( 43.01140435219951996, 2.710499672648754466, 34.21067981925357060 ) ) ;
#7220 = CARTESIAN_POINT ( 'NONE',  ( 39.42975644700377558, 87.67977050742732104, 36.81289934271958941 ) ) ;
#7221 = CARTESIAN_POINT ( 'NONE',  ( -154.3824083646099439, -166.2938272943107165, 58.62277379824867296 ) ) ;
#7222 = AXIS2_PLACEMENT_3D ( 'NONE', #4168, #9140, #10897 ) ;
#7223 = CARTESIAN_POINT ( 'NONE',  ( 46.59305225739526435, 76.91518717409400097, 31.60846029578754468 ) ) ;
#7224 = DIRECTION ( 'NONE',  ( -0.000000000000000000, -0.000000000000000000, -1.000000000000000000 ) ) ;
#7225 = DIRECTION ( 'NONE',  ( -0.000000000000000000, -0.000000000000000000, -1.000000000000000000 ) ) ;
#7226 = VERTEX_POINT ( 'NONE', #4958 ) ;
#7227 = CARTESIAN_POINT ( 'NONE',  ( 43.01140435219951286, 69.53445800887257633, 39.21067981925356349 ) ) ;
#7228 = ADVANCED_FACE ( 'NONE', ( #6499 ), #12566, .F. ) ;
#7229 = CARTESIAN_POINT ( 'NONE',  ( 43.01140435219951996, 10.71049967264875491, 34.21067981925357060 ) ) ;
#7230 = CARTESIAN_POINT ( 'NONE',  ( 40.27526882409969744, 129.8297705074273267, 37.97664729208901235 ) ) ;
#7231 = CARTESIAN_POINT ( 'NONE',  ( 76.07019559177007295, 111.3280993686123281, -14.13269547130637704 ) ) ;
#7232 = VERTEX_POINT ( 'NONE', #18290 ) ;
#7233 = SURFACE_STYLE_FILL_AREA ( #17235 ) ;
#7234 = ORIENTED_EDGE ( 'NONE', *, *, #21469, .F. ) ;
#7235 = CARTESIAN_POINT ( 'NONE',  ( 39.42975644700377558, 138.0797705074273267, 31.60846029578754468 ) ) ;
#7236 = CARTESIAN_POINT ( 'NONE',  ( -145.2889157411863437, -180.5391397928654555, 41.15050349809589392 ) ) ;
#7237 = CARTESIAN_POINT ( 'NONE',  ( 39.92123440845005433, 111.2344580088725650, 38.46393386101375711 ) ) ;
#7238 = CARTESIAN_POINT ( 'NONE',  ( -153.0531000319306827, -168.8899795514095672, 59.65701158161631668 ) ) ;
#7239 = CARTESIAN_POINT ( 'NONE',  ( -143.3790856849358306, -191.7630981290893146, 43.77915905869157598 ) ) ;
#7240 = CARTESIAN_POINT ( 'NONE',  ( 46.59305225739526435, 97.31518717409400665, 36.81289934271958941 ) ) ;
#7241 = CARTESIAN_POINT ( 'NONE',  ( -142.0420953463935803, -156.2438272943106767, 46.59394152635518083 ) ) ;
#7242 = CARTESIAN_POINT ( 'NONE',  ( 136.2768881589198600, 181.8432453435729883, 21.97307119874763259 ) ) ;
#7243 = CARTESIAN_POINT ( 'NONE',  ( -143.3790856849358306, -158.7630981290893146, 43.77915905869157598 ) ) ;
#7244 = DIRECTION ( 'NONE',  ( 1.000000000000000000, 0.000000000000000000, 0.000000000000000000 ) ) ;
#7245 = VECTOR ( 'NONE', #5157, 1000.000000000000227 ) ;
#7246 = EDGE_CURVE ( 'NONE', #17093, #1584, #19631, .T. ) ;
#7247 = CARTESIAN_POINT ( 'NONE',  ( 46.10157429594899270, 141.8344580088725593, 38.46393386101376421 ) ) ;
#7248 = CARTESIAN_POINT ( 'NONE',  ( 45.74753988029933538, 115.4297705074272926, 37.97664729208901946 ) ) ;
#7249 = CARTESIAN_POINT ( 'NONE',  ( 31.11878897118147336, 145.5659923423516773, -4.562434011626001151 ) ) ;
#7250 = CARTESIAN_POINT ( 'NONE',  ( -141.4692556286852891, -183.8391397928654669, 46.40781461928724383 ) ) ;
#7251 = CARTESIAN_POINT ( 'NONE',  ( 38.58424406990785371, 107.9651871740939981, 32.77220824515697473 ) ) ;
#7252 = ORIENTED_EDGE ( 'NONE', *, *, #9356, .F. ) ;
#7253 = CARTESIAN_POINT ( 'NONE',  ( 46.10157429594899270, 156.8344580088725593, 38.46393386101375711 ) ) ;
#7254 = CARTESIAN_POINT ( 'NONE',  ( 11.74529739132928619, 133.8467647624810581, -4.446451035385589279 ) ) ;
#7255 = CARTESIAN_POINT ( 'NONE',  ( 35.91077447413180579, 147.1981228300969633, 10.63281669705329691 ) ) ;
#7256 = PLANE ( 'NONE',  #12855 ) ;
#7257 = CARTESIAN_POINT ( 'NONE',  ( 47.43856463449118621, 73.87977050742732388, 34.21067981925357060 ) ) ;
#7258 = ORIENTED_EDGE ( 'NONE', *, *, #4029, .T. ) ;
#7259 = CARTESIAN_POINT ( 'NONE',  ( 44.55648932407425633, 67.88445800887258486, 29.45539723777780239 ) ) ;
#7260 = B_SPLINE_CURVE_WITH_KNOTS ( 'NONE', 3,
 ( #6207, #20430, #1585, #13377, #16891, #15023, #10295, #1805, #15250, #148, #5005, #4888, #6547, #20324, #18337, #16786, #8640, #5222, #11609, #11938, #15362, #253, #18666, #5325, #10403, #16673, #12042, #13270, #18772, #17103, #18560, #20005, #18450, #1698, #2019, #8427, #21763, #3239, #8750, #9970, #8315, #20114, #11715, #3349, #15136, #39, #6779, #13486, #20218, #5111, #11828, #17321, #7202, #19203, #12362, #15879, #2441, #2231, #793, #8859, #12585, #7527, #15668, #19309, #14228, #9182, #18988, #9071, #20968, #10723, #15566, #20859, #7315, #8961, #10511, #14016, #12256, #5855, #10834, #4100, #9287, #4206, #571, #10935, #469, #17643, #368, #19101, #2550, #20751, #13801, #13905, #14120, #3891, #7096, #5424, #685, #5640, #2333, #3998, #15779, #10614, #20538, #17532, #12141, #17425, #18875, #3782, #7421, #5748, #17208, #2123, #20644, #12472, #5527, #13024, #21082, #4310, #14665, #19412, #18193, #11034, #17749, #9395, #1336, #19744, #4639, #2652, #6179, #11464, #19856, #4744, #7749, #11357, #18080, #2986, #6292, #3100, #16100, #9725, #15987, #11143, #6073, #16424, #898, #1012, #8069, #1119, #16316, #5964, #14776, #12690, #21518, #1226, #7639, #6405, #14555, #7853, #13130, #14341, #14448, #21185 ),
 .UNSPECIFIED., .F., .F.,
 ( 4, 2, 2, 2, 2, 2, 2, 2, 2, 2, 2, 2, 2, 2, 2, 2, 2, 2, 2, 2, 2, 2, 2, 2, 2, 2, 2, 2, 2, 2, 2, 2, 2, 2, 2, 2, 2, 2, 2, 2, 2, 2, 2, 2, 2, 2, 2, 2, 2, 2, 2, 2, 2, 2, 2, 2, 2, 2, 2, 2, 2, 2, 2, 2, 2, 2, 2, 2, 2, 2, 2, 2, 2, 2, 2, 2, 2, 2, 2, 2, 4 ),
 ( 0.000000000000000000, 0.008318061648474830982, 0.01871563870907547167, 0.02911321576967611582, 0.03951079283027675998, 0.04990836989087740067, 0.06030594695147804829, 0.07070352401207868898, 0.08110110107267932966, 0.09149867813327997035, 0.1018962551938806110, 0.1122938322544812378, 0.1226914093150818785, 0.1330889863756825053, 0.1434865634362831321, 0.1538841404968837590, 0.1642817175574844135, 0.1746792946180850126, 0.1850768716786856394, 0.1954744487392862939, 0.2058720257998869485, 0.2162696028604875753, 0.2266671799210882021, 0.2370647569816888289, 0.2474623340422894557, 0.2578599111028900825, 0.2682574881634907094, 0.2786550652240913362, 0.2890526422846919630, 0.2994502193452925343, 0.3098477964058931611, 0.3202453734664938434, 0.3306429505270944147, 0.3410405275876950415, 0.3514381046482956683, 0.3618356817088962951, 0.3722332587694969219, 0.3826308358300975487, 0.3930284128906983421, 0.4034259899512990799, 0.4138235670118998732, 0.4242211440725006666, 0.4346187211331003497, 0.4450162981936999218, 0.4554138752542995494, 0.4658114523148991770, 0.4762090293755007475, 0.4866066064361022070, 0.4970041834967036110, 0.5074017605573051259, 0.5177993376179057528, 0.5281969146785063796, 0.5385944917391070064, 0.5489920687997077442, 0.5593896458603083710, 0.5697872229209089978, 0.5801847999815096246, 0.5905823770421102514, 0.6009799541027108782, 0.6113775311633115050, 0.6217751082239121319, 0.6321726852845127587, 0.6425702623451133855, 0.6529678394057140123, 0.6633654164663146391, 0.6737629935269153769, 0.6841605705875142274, 0.6945581476481129668, 0.7049557247087120393, 0.7153533017693110008, 0.7257508788299132929, 0.7361484558905155851, 0.7465460329511179882, 0.7569436100117202804, 0.7673411870723210182, 0.7777387641329215340, 0.7881363411935222718, 0.7985339182541228986, 0.8080132075800156022, 0.8174924969059083057, 0.8280181261579530050 ),
 .UNSPECIFIED. ) ;
#7261 = AXIS2_PLACEMENT_3D ( 'NONE', #13926, #10316, #20665 ) ;
#7262 = CARTESIAN_POINT ( 'NONE',  ( 48.01140435219951996, 131.0604996726487457, 35.83527830041810347 ) ) ;
#7264 = CARTESIAN_POINT ( 'NONE',  ( 73.15003751907750029, 103.8404476760371864, -6.870911935119222491 ) ) ;
#7263 = CARTESIAN_POINT ( 'NONE',  ( 39.42975644700377558, 84.41518717409400097, 36.81289934271958941 ) ) ;
#7265 = EDGE_CURVE ( 'NONE', #16287, #5105, #18404, .T. ) ;
#7266 = CARTESIAN_POINT ( 'NONE',  ( -160.8964159109769696, -184.7438272943107052, 52.72008163687743121 ) ) ;
#7267 = CARTESIAN_POINT ( 'NONE',  ( 38.96631938032478359, 117.0844580088725877, 37.14960608071593384 ) ) ;
#7268 = CARTESIAN_POINT ( 'NONE',  ( 48.01140435219951996, 127.1344580088725706, 35.83527830041809636 ) ) ;
#7269 =( NAMED_UNIT ( * ) SI_UNIT ( $, .STERADIAN. ) SOLID_ANGLE_UNIT ( ) );
#7270 = CARTESIAN_POINT ( 'NONE',  ( 41.46631938032478359, 93.38445800887258486, 38.96596240072933170 ) ) ;
#7271 = CARTESIAN_POINT ( 'NONE',  ( 40.27526882409969033, 138.8297705074272983, 37.97664729208901946 ) ) ;
#7272 = CARTESIAN_POINT ( 'NONE',  ( 39.42975644700377558, 108.0797705074273125, 31.60846029578754468 ) ) ;
#7273 = CARTESIAN_POINT ( 'NONE',  ( 8.798315742295939046, 121.0924013121165075, 9.124689178586496752 ) ) ;
#7274 = CARTESIAN_POINT ( 'NONE',  ( 45.74753988029934249, 133.1651871740940010, 37.97664729208901235 ) ) ;
#7275 = CIRCLE ( 'NONE', #19574, 10.00000000000000888 ) ;
#7276 = DIRECTION ( 'NONE',  ( 0.000000000000000000, -0.000000000000000000, 1.000000000000000000 ) ) ;
#7277 = CARTESIAN_POINT ( 'NONE',  ( -157.2955611005345986, -161.6084106276440480, 41.63779006702063867 ) ) ;
#7278 = CARTESIAN_POINT ( 'NONE',  ( -161.4692556286852891, -164.3391397928654385, 52.90620854394536821 ) ) ;
#7279 = AXIS2_PLACEMENT_3D ( 'NONE', #21086, #8862, #14019 ) ;
#7280 = CARTESIAN_POINT ( 'NONE',  ( 31.20897972572456069, 148.4098837309091721, 17.43780275515692679 ) ) ;
#7281 = EDGE_CURVE ( 'NONE', #21028, #12248, #64, .T. ) ;
#7282 = CARTESIAN_POINT ( 'NONE',  ( 68.16012629694054681, 106.9699110742356396, 5.199846382127304878 ) ) ;
#7283 = DIRECTION ( 'NONE',  ( 0.000000000000000000, 0.000000000000000000, 1.000000000000000000 ) ) ;
#7284 = CARTESIAN_POINT ( 'NONE',  ( 41.64333658814960870, 117.7151871740939981, 38.42115945441014446 ) ) ;
#7285 =( BOUNDED_CURVE ( )  B_SPLINE_CURVE ( 2, ( #10838, #473, #15991, #17429, #19312, #4210, #19416, #2553, #9075, #2337, #9290, #7643, #10939 ),
 .UNSPECIFIED., .F., .F. ) 
 B_SPLINE_CURVE_WITH_KNOTS ( ( 3, 2, 2, 2, 2, 2, 3 ),
 ( 0.8161764705882352811, 0.8176470588235293935, 0.8205882352941176183, 0.8235294117647058432, 0.8264705882352940680, 0.8294117647058824039, 0.8308823529411765163 ),
 .UNSPECIFIED. ) 
 CURVE ( )  GEOMETRIC_REPRESENTATION_ITEM ( )  RATIONAL_B_SPLINE_CURVE ( ( 0.9755282581475768211, 0.9755282581475768211, 1.000000000000000000, 0.9510565162951535312, 1.000000000000000000, 0.9510565162951535312, 1.000000000000000000, 0.9510565162951535312, 1.000000000000000000, 0.9510565162951535312, 1.000000000000000000, 0.9755282581475768211, 0.9755282581475768211 ) ) 
 REPRESENTATION_ITEM ( '' )  );
#7286 = EDGE_LOOP ( 'NONE', ( #5962, #20428, #7396, #2232 ) ) ;
#7287 = VECTOR ( 'NONE', #3110, 1000.000000000000000 ) ;
#7288 = CARTESIAN_POINT ( 'NONE',  ( -159.5594255724347761, -160.8630981290893089, 43.77915905869157598 ) ) ;
#7289 = VERTEX_POINT ( 'NONE', #18172 ) ;
#7290 = CARTESIAN_POINT ( 'NONE',  ( 43.01140435219951286, 105.5344580088725621, 39.46799094044489209 ) ) ;
#7291 = VECTOR ( 'NONE', #1941, 999.9999999999998863 ) ;
#7292 = CARTESIAN_POINT ( 'NONE',  ( 39.42975644700377558, 150.0797705074273267, 31.60846029578754468 ) ) ;
#7293 = CARTESIAN_POINT ( 'NONE',  ( 45.74753988029933538, 61.42977050742732104, 37.97664729208901946 ) ) ;
#7295 = CARTESIAN_POINT ( 'NONE',  ( 15.80414578680225723, 112.4924633436790344, 15.87081086175909306 ) ) ;
#7294 = CARTESIAN_POINT ( 'NONE',  ( 46.59305225739526435, 115.3151871740940067, 36.81289934271958941 ) ) ;
#7296 = VECTOR ( 'NONE', #21107, 1000.000000000000000 ) ;
#7297 = CARTESIAN_POINT ( 'NONE',  ( 39.92123440845004723, 72.26049967264870588, 29.95742577749337343 ) ) ;
#7299 = LINE ( 'NONE', #12344, #9017 ) ;
#7298 = DIRECTION ( 'NONE',  ( -0.3450121214752275844, 0.9385982292947088190, 0.000000000000000000 ) ) ;
#7300 = CARTESIAN_POINT ( 'NONE',  ( 38.01140435219952707, 71.93445800887258201, 35.83527830041809636 ) ) ;
#7301 = CARTESIAN_POINT ( 'NONE',  ( 47.75598903798131545, 95.36109484030878036, 32.59926919370181508 ) ) ;
#7302 = CARTESIAN_POINT ( 'NONE',  ( 43.01140435219951996, 10.71049967264875491, 29.21067981925357060 ) ) ;
#7303 = CARTESIAN_POINT ( 'NONE',  ( -148.5561028927606344, -180.9938272943107336, 58.62277379824867296 ) ) ;
#7304 = CARTESIAN_POINT ( 'NONE',  ( -160.8964159109769696, -191.0084106276440536, 52.72008163687743121 ) ) ;
#7305 = VERTEX_POINT ( 'NONE', #13004 ) ;
#7306 = ADVANCED_FACE ( 'NONE', ( #3193 ), #8380, .T. ) ;
#7307 = CARTESIAN_POINT ( 'NONE',  ( -160.8964159109769696, -176.1584106276440309, 49.65701158161630957 ) ) ;
#7308 = CARTESIAN_POINT ( 'NONE',  ( 26.67903320394502131, 150.0857490671680807, 9.287084330314211655 ) ) ;
#7309 = ORIENTED_EDGE ( 'NONE', *, *, #8399, .F. ) ;
#7310 = CARTESIAN_POINT ( 'NONE',  ( 38.58424406990786082, 144.1151871740939896, 34.21067981925357060 ) ) ;
#7311 = DIRECTION ( 'NONE',  ( 0.7066505893342458489, 0.7066505893340067068, 0.03591502732094190020 ) ) ;
#7312 = CARTESIAN_POINT ( 'NONE',  ( 47.43856463449117911, 101.0297705074273154, 32.77220824515697473 ) ) ;
#7313 = CARTESIAN_POINT ( 'NONE',  ( 9.656473946750173454, 127.6128973189080398, 2.339233609801092406 ) ) ;
#7314 = VERTEX_POINT ( 'NONE', #13114 ) ;
#7315 = CARTESIAN_POINT ( 'NONE',  ( 17.20459894546975832, 108.5405110446994001, 1.704077971530460811 ) ) ;
#7316 = EDGE_CURVE ( 'NONE', #255, #11879, #6384, .T. ) ;
#7317 = ORIENTED_EDGE ( 'NONE', *, *, #10231, .F. ) ;
#7318 = CARTESIAN_POINT ( 'NONE',  ( 44.37947211624943833, 110.4797705074273324, 30.00020018409699318 ) ) ;
#7319 = VECTOR ( 'NONE', #13142, 1000.000000000000000 ) ;
#7320 = DIRECTION ( 'NONE',  ( 0.000000000000000000, 0.000000000000000000, -1.000000000000000000 ) ) ;
#7321 = CARTESIAN_POINT ( 'NONE',  ( 43.01140435219951286, 147.8651871740940180, 38.86567161673127657 ) ) ;
#7322 = CARTESIAN_POINT ( 'NONE',  ( 38.01140435219951996, 96.56049967264871725, 32.58608133808903773 ) ) ;
#7323 = CARTESIAN_POINT ( 'NONE',  ( 15.39564893635072806, 140.1373336744895255, -4.208549045858890558 ) ) ;
#7324 = CARTESIAN_POINT ( 'NONE',  ( -151.4692556286852891, -196.9891397928655010, 49.65701158161630957 ) ) ;
#7325 = CARTESIAN_POINT ( 'NONE',  ( -154.5594255724347761, -174.0891397928654669, 40.14644641866476604 ) ) ;
#7326 = EDGE_CURVE ( 'NONE', #14746, #11386, #11446, .T. ) ;
#7327 = PLANE ( 'NONE',  #2721 ) ;
#7328 = CARTESIAN_POINT ( 'NONE',  ( 47.05648932407426344, 64.58445800887258770, 31.27175355779120025 ) ) ;
#7329 = DIRECTION ( 'NONE',  ( -0.000000000000000000, -0.000000000000000000, -1.000000000000000000 ) ) ;
#7330 = ORIENTED_EDGE ( 'NONE', *, *, #20404, .F. ) ;
#7331 = CARTESIAN_POINT ( 'NONE',  ( 46.59305225739526435, 80.17977050742732104, 31.60846029578754468 ) ) ;
#7332 = CARTESIAN_POINT ( 'NONE',  ( -154.3824083646099439, -167.4938272943107336, 40.69124936498395328 ) ) ;
#7333 = CARTESIAN_POINT ( 'NONE',  ( 46.59305225739526435, 82.31518717409400665, 36.81289934271958941 ) ) ;
#7335 = AXIS2_PLACEMENT_3D ( 'NONE', #8477, #17042, #11760 ) ;
#7334 = CARTESIAN_POINT ( 'NONE',  ( 33.56091001181424360, 87.00402361476987778, -6.351118090676544981 ) ) ;
#7336 = DIRECTION ( 'NONE',  ( 0.000000000000000000, 0.000000000000000000, -1.000000000000000000 ) ) ;
#7337 = EDGE_LOOP ( 'NONE', ( #4458, #6519, #12463, #12605 ) ) ;
#7338 = CARTESIAN_POINT ( 'NONE',  ( -151.4692556286852891, -126.9891397928655010, -44.65701158161626694 ) ) ;
#7339 = DIRECTION ( 'NONE',  ( -0.8302490056034136368, -0.5573926701119623628, 9.854660648260997410E-17 ) ) ;
#7340 = CARTESIAN_POINT ( 'NONE',  ( 38.58424406990785371, 132.2297705074273040, 32.77220824515697473 ) ) ;
#7341 = CARTESIAN_POINT ( 'NONE',  ( 48.12388674207330297, 92.25590008057444891, 8.208355790051324874 ) ) ;
#7342 = ORIENTED_EDGE ( 'NONE', *, *, #5733, .T. ) ;
#7343 = PLANE ( 'NONE',  #590 ) ;
#7344 = ORIENTED_EDGE ( 'NONE', *, *, #16894, .T. ) ;
#7345 = CARTESIAN_POINT ( 'NONE',  ( -120.0322075325610740, -126.9891397928655010, 30.00000000000000000 ) ) ;
#7346 = CARTESIAN_POINT ( 'NONE',  ( 46.10157429594899270, 121.7344580088725934, 29.95742577749336988 ) ) ;
#7347 = CARTESIAN_POINT ( 'NONE',  ( -148.3790856849358306, -194.4630981290893317, 40.14644641866477315 ) ) ;
#7348 = EDGE_CURVE ( 'NONE', #14309, #10265, #16864, .T. ) ;
#7349 = CARTESIAN_POINT ( 'NONE',  ( 46.59305225739526435, 100.9151871740940010, 31.60846029578754468 ) ) ;
#7350 = CARTESIAN_POINT ( 'NONE',  ( 47.05648932407426344, 133.5844580088725877, 31.27175355779120025 ) ) ;
#7351 = CARTESIAN_POINT ( 'NONE',  ( -159.5594255724347761, -163.2630981290893146, 55.53486410454104316 ) ) ;
#7352 = CARTESIAN_POINT ( 'NONE',  ( 299.3480347479280681, 0.000000000000000000, -2.775557561562891351E-14 ) ) ;
#7353 = LINE ( 'NONE', #12405, #1923 ) ;
#7354 = CARTESIAN_POINT ( 'NONE',  ( 38.01140435219951996, 131.6344580088725991, 32.58608133808903773 ) ) ;
#7355 = CARTESIAN_POINT ( 'NONE',  ( 45.74753988029933538, 112.4297705074273210, 37.97664729208901946 ) ) ;
#7356 = CARTESIAN_POINT ( 'NONE',  ( 52.07920593110389262, 93.11959619657488929, 13.05671643426689776 ) ) ;
#7357 = CARTESIAN_POINT ( 'NONE',  ( -160.8964159109769696, -190.8938272943107393, 49.65701158161630957 ) ) ;
#7358 = CARTESIAN_POINT ( 'NONE',  ( 44.37947211624943833, 104.2151871740939981, 30.00020018409699318 ) ) ;
#7359 = CARTESIAN_POINT ( 'NONE',  ( -145.2889157411863437, -162.5130981290893430, 58.16351966513671812 ) ) ;
#7360 = ORIENTED_EDGE ( 'NONE', *, *, #20527, .T. ) ;
#7361 = CARTESIAN_POINT ( 'NONE',  ( 44.55648932407425633, 75.68445800887258201, 38.96596240072933170 ) ) ;
#7362 = CARTESIAN_POINT ( 'NONE',  ( 75.85495621331871519, 129.5603373922052697, -8.732165470513974626 ) ) ;
#7363 = EDGE_CURVE ( 'NONE', #13378, #13154, #7385, .T. ) ;
#7364 = CARTESIAN_POINT ( 'NONE',  ( 54.67410106651116308, 94.23276814491528341, 6.942135068398441078 ) ) ;
#7365 = DIRECTION ( 'NONE',  ( 0.000000000000000000, 0.000000000000000000, 1.000000000000000000 ) ) ;
#7366 = CARTESIAN_POINT ( 'NONE',  ( 39.42975644700377558, 72.67977050742730682, 36.81289934271958941 ) ) ;
#7367 = EDGE_LOOP ( 'NONE', ( #546, #20132, #4048, #6071, #17857, #3320, #12825, #9669, #6290, #1145, #17255, #14311, #897, #16422, #7903, #18191, #16039, #19712, #14097, #5799, #794, #7503, #11549, #17880, #6985, #242, #2906, #11708, #17859, #8389, #13474 ) ) ;
#7368 = EDGE_CURVE ( 'NONE', #16674, #21451, #9082, .T. ) ;
#7369 = CIRCLE ( 'NONE', #1376, 10.00000000000000888 ) ;
#7370 = CARTESIAN_POINT ( 'NONE',  ( 47.05648932407426344, 60.98445800887257207, 37.14960608071593384 ) ) ;
#7371 = CARTESIAN_POINT ( 'NONE',  ( -149.8854112254399240, -171.3160212151857138, 39.65701158161629536 ) ) ;
#7372 = CARTESIAN_POINT ( 'NONE',  ( 41.46631938032478359, 124.3104996726487457, 38.96596240072933170 ) ) ;
#7374 = CARTESIAN_POINT ( 'NONE',  ( 73.74613032677598312, 134.8023270448005064, -0.9181577650121128809 ) ) ;
#7373 = CARTESIAN_POINT ( 'NONE',  ( 43.01140435219951286, 78.86518717409400381, 38.86567161673127657 ) ) ;
#7375 = CARTESIAN_POINT ( 'NONE',  ( -142.0420953463936087, -180.3938272943107108, 49.65701158161630957 ) ) ;
#7376 = CARTESIAN_POINT ( 'NONE',  ( 75.40436159597490473, 130.9804297329818326, 12.22031048084446248 ) ) ;
#7377 = CARTESIAN_POINT ( 'NONE',  ( -154.5594255724347761, -191.1630981290893203, 40.14644641866476604 ) ) ;
#7378 =( NAMED_UNIT ( * ) PLANE_ANGLE_UNIT ( ) SI_UNIT ( $, .RADIAN. ) );
#7379 = DIRECTION ( 'NONE',  ( 0.000000000000000000, 0.000000000000000000, 1.000000000000000000 ) ) ;
#7380 = CARTESIAN_POINT ( 'NONE',  ( -149.8854112254399240, -162.3160212151857138, 39.65701158161629536 ) ) ;
#7381 = CARTESIAN_POINT ( 'NONE',  ( 44.37947211624943833, 145.2797705074273154, 38.42115945441014446 ) ) ;
#7382 = CARTESIAN_POINT ( 'NONE',  ( 46.59305225739526435, 107.1797705074273352, 31.60846029578754468 ) ) ;
#7383 = CARTESIAN_POINT ( 'NONE',  ( 52.46025766099742071, 152.8098426157893925, 11.14871012209260748 ) ) ;
#7384 = CARTESIAN_POINT ( 'NONE',  ( 45.74753988029934249, 139.1651871740940010, 37.97664729208901235 ) ) ;
#7385 = CIRCLE ( 'NONE', #2786, 21.90454335994848734 ) ;
#7386 = CARTESIAN_POINT ( 'NONE',  ( -143.8425227516148084, -156.6938272943107222, 55.19815736654470584 ) ) ;
#7387 = CARTESIAN_POINT ( 'NONE',  ( -154.3824083646099439, -163.5584106276440366, 58.62277379824867296 ) ) ;
#7388 =( GEOMETRIC_REPRESENTATION_CONTEXT ( 3 ) GLOBAL_UNCERTAINTY_ASSIGNED_CONTEXT ( ( #2663 ) ) GLOBAL_UNIT_ASSIGNED_CONTEXT ( ( #12101, #3953, #14187 ) ) REPRESENTATION_CONTEXT ( 'NONE', 'WORKASPACE' ) );
#7389 = DIRECTION ( 'NONE',  ( 1.000000000000000000, 0.000000000000000000, 0.000000000000000000 ) ) ;
#7390 = PLANE ( 'NONE',  #20158 ) ;
#7391 = CARTESIAN_POINT ( 'NONE',  ( 32.24825037804825456, 146.0601464669000791, 9.485560667832931614 ) ) ;
#7392 = CARTESIAN_POINT ( 'NONE',  ( 45.74753988029933538, 115.1651871740940010, 37.97664729208901946 ) ) ;
#7393 = ORIENTED_EDGE ( 'NONE', *, *, #1462, .F. ) ;
#7394 = ADVANCED_FACE ( 'NONE', ( #6944 ), #13543, .T. ) ;
#7395 = CARTESIAN_POINT ( 'NONE',  ( -157.6495955161842062, -179.0391397928654840, 58.16351966513671812 ) ) ;
#7396 = ORIENTED_EDGE ( 'NONE', *, *, #20255, .T. ) ;
#7397 = CARTESIAN_POINT ( 'NONE',  ( 46.10157429594899270, 88.73445800887256496, 29.95742577749337343 ) ) ;
#7398 = COLOUR_RGB ( '', 0.09019608, 0.27058824, 0.51372549) ;
#7399 = CARTESIAN_POINT ( 'NONE',  ( 48.01140435219951996, 155.2104996726487514, 34.21067981925357060 ) ) ;
#7401 = CARTESIAN_POINT ( 'NONE',  ( 63.17392202723403472, 139.5086487405075673, -1.196242060499778992 ) ) ;
#7400 = CARTESIAN_POINT ( 'NONE',  ( 43.01140435219951286, 104.3651871740940038, 29.55568802177586463 ) ) ;
#7402 = CARTESIAN_POINT ( 'NONE',  ( 41.46631938032478359, 76.31049967264874567, 38.96596240072933170 ) ) ;
#7404 = CARTESIAN_POINT ( 'NONE',  ( -159.5594255724347761, -157.2630981290893146, 55.53486410454104316 ) ) ;
#7403 = DIRECTION ( 'NONE',  ( -0.3450121214752278065, 0.9385982292947087080, 0.000000000000000000 ) ) ;
#7405 = FACE_OUTER_BOUND ( 'NONE', #6873, .T. ) ;
#7406 = CARTESIAN_POINT ( 'NONE',  ( 44.62452158104316879, 94.95733355596098590, 29.46674713776154775 ) ) ;
#7407 = CARTESIAN_POINT ( 'NONE',  ( 44.37947211624943833, 71.21518717409399812, 30.00020018409699318 ) ) ;
#7408 = CARTESIAN_POINT ( 'NONE',  ( 76.17254549292280785, -61.68114226949890622, -16.21320343559643717 ) ) ;
#7409 = CARTESIAN_POINT ( 'NONE',  ( -157.2955611005346270, -179.3438272943107279, 41.63779006702063867 ) ) ;
#7410 = CARTESIAN_POINT ( 'NONE',  ( -143.8425227516148084, -189.9584106276440423, 55.19815736654470584 ) ) ;
#7411 = ORIENTED_EDGE ( 'NONE', *, *, #20563, .F. ) ;
#7412 =( BOUNDED_CURVE ( )  B_SPLINE_CURVE ( 2, ( #18530, #10266, #20192, #18310, #15223, #16755, #11688, #19977, #1666, #21734, #11909, #5191, #18637 ),
 .UNSPECIFIED., .F., .T. ) 
 B_SPLINE_CURVE_WITH_KNOTS ( ( 3, 2, 2, 2, 2, 2, 3 ),
 ( 0.1102941176470588203, 0.1117647058823529466, 0.1147058823529411714, 0.1176470588235294101, 0.1205882352941176489, 0.1235294117647058876, 0.1249999999999999861 ),
 .UNSPECIFIED. ) 
 CURVE ( )  GEOMETRIC_REPRESENTATION_ITEM ( )  RATIONAL_B_SPLINE_CURVE ( ( 0.9755282581475767101, 0.9755282581475765991, 1.000000000000000000, 0.9510565162951535312, 1.000000000000000000, 0.9510565162951535312, 1.000000000000000000, 0.9510565162951535312, 1.000000000000000000, 0.9510565162951535312, 1.000000000000000000, 0.9755282581475769321, 0.9755282581475765991 ) ) 
 REPRESENTATION_ITEM ( '' )  );
#7413 = CARTESIAN_POINT ( 'NONE',  ( -145.6429501568359797, -175.1084106276440480, 57.67623309621198047 ) ) ;
#7414 = CARTESIAN_POINT ( 'NONE',  ( 23.80922038702690102, 91.46939207759763235, 0.001460074241615882690 ) ) ;
#7415 = ORIENTED_EDGE ( 'NONE', *, *, #12686, .T. ) ;
#7416 = CARTESIAN_POINT ( 'NONE',  ( 40.27526882409969033, 144.5651871740939782, 37.97664729208901946 ) ) ;
#7417 =( GEOMETRIC_REPRESENTATION_CONTEXT ( 3 ) GLOBAL_UNCERTAINTY_ASSIGNED_CONTEXT ( ( #3112 ) ) GLOBAL_UNIT_ASSIGNED_CONTEXT ( ( #15176, #3388, #11536 ) ) REPRESENTATION_CONTEXT ( 'NONE', 'WORKASPACE' ) );
#7418 = CARTESIAN_POINT ( 'NONE',  ( 39.42975644700377558, 108.0797705074273125, 31.60846029578754468 ) ) ;
#7419 = ORIENTED_EDGE ( 'NONE', *, *, #6661, .F. ) ;
#7420 = ORIENTED_EDGE ( 'NONE', *, *, #2520, .T. ) ;
#7421 = CARTESIAN_POINT ( 'NONE',  ( 26.10333545525518062, 97.33820528946348816, 8.132564544556878161 ) ) ;
#7422 = VERTEX_POINT ( 'NONE', #5171 ) ;
#7423 = CARTESIAN_POINT ( 'NONE',  ( 38.96631938032478359, 117.0844580088725877, 37.14960608071593384 ) ) ;
#7424 = DIRECTION ( 'NONE',  ( 1.000000000000000000, 0.000000000000000000, 0.000000000000000000 ) ) ;
#7425 = CARTESIAN_POINT ( 'NONE',  ( 38.58424406990784661, 84.22977050742730398, 32.77220824515698183 ) ) ;
#7426 = CARTESIAN_POINT ( 'NONE',  ( 40.27526882409969033, 141.5651871740940067, 37.97664729208901946 ) ) ;
#7427 = CARTESIAN_POINT ( 'NONE',  ( 38.01140435219952707, 102.7104996726487514, 34.21067981925357060 ) ) ;
#7428 = CARTESIAN_POINT ( 'NONE',  ( 76.81974253126139729, 125.2811442093199616, -1.589308178208348910 ) ) ;
#7429 = CARTESIAN_POINT ( 'NONE',  ( -157.6495955161842062, -170.0391397928654840, 58.16351966513671812 ) ) ;
#7430 = CARTESIAN_POINT ( 'NONE',  ( -141.4692556286852891, -158.9130981290892919, 46.40781461928724383 ) ) ;
#7431 = CARTESIAN_POINT ( 'NONE',  ( -138.5468111011521160, 759.4679229819337252, -0.8325491102011938205 ) ) ;
#7432 = DIRECTION ( 'NONE',  ( -0.5000000000000003331, 0.000000000000000000, 0.8660254037844384856 ) ) ;
#7433 = ORIENTED_EDGE ( 'NONE', *, *, #7932, .T. ) ;
#7434 = CARTESIAN_POINT ( 'NONE',  ( 47.43856463449117200, 82.72977050742731819, 35.64915139335016647 ) ) ;
#7435 = CARTESIAN_POINT ( 'NONE',  ( -145.6429501568359797, -167.9438272943107506, 41.63779006702063867 ) ) ;
#7436 = CARTESIAN_POINT ( 'NONE',  ( 44.37947211624943833, 67.01518717409399528, 38.42115945441014446 ) ) ;
#7437 = CARTESIAN_POINT ( 'NONE',  ( 15.39564893635072806, 140.1373336744895255, -4.208549045858890558 ) ) ;
#7438 = CARTESIAN_POINT ( 'NONE',  ( -142.0420953463936087, -192.6584106276440593, 49.65701158161630957 ) ) ;
#7439 = VERTEX_POINT ( 'NONE', #11891 ) ;
#7440 = PLANE ( 'NONE',  #12589 ) ;
#7441 = CARTESIAN_POINT ( 'NONE',  ( 43.01140435219951996, 10.71049967264875491, 34.21067981925357060 ) ) ;
#7442 = CARTESIAN_POINT ( 'NONE',  ( 38.58424406990785371, 138.2297705074273324, 32.77220824515697473 ) ) ;
#7443 = CARTESIAN_POINT ( 'NONE',  ( 60.64192606672164487, 149.1585417170215067, -15.56126092485307488 ) ) ;
#7444 = ORIENTED_EDGE ( 'NONE', *, *, #15000, .T. ) ;
#7445 = DIRECTION ( 'NONE',  ( 1.000000000000000000, 0.000000000000000000, -0.000000000000000000 ) ) ;
#7446 = ORIENTED_EDGE ( 'NONE', *, *, #12478, .F. ) ;
#7447 = CARTESIAN_POINT ( 'NONE',  ( 47.43856463449117200, 125.0297705074273011, 32.77220824515698183 ) ) ;
#7448 = CARTESIAN_POINT ( 'NONE',  ( 47.05648932407426344, 138.9844580088725650, 37.14960608071593384 ) ) ;
#7449 = CARTESIAN_POINT ( 'NONE',  ( 48.01140435219951996, 155.0604996726487457, 35.83527830041809636 ) ) ;
#7450 = FACE_OUTER_BOUND ( 'NONE', #16031, .T. ) ;
#7451 = CARTESIAN_POINT ( 'NONE',  ( -97.23064952102208736, 13.78046159333444720, -19.99999999999997868 ) ) ;
#7452 = CARTESIAN_POINT ( 'NONE',  ( 163.2639715594360155, 191.9628544139417841, 23.38668371770654275 ) ) ;
#7453 = CARTESIAN_POINT ( 'NONE',  ( 43.01140435219951286, 101.3651871740939896, 29.55568802177586463 ) ) ;
#7454 = CARTESIAN_POINT ( 'NONE',  ( 43.01140435219951286, 134.0344580088725763, 29.21067981925356705 ) ) ;
#7455 = CARTESIAN_POINT ( 'NONE',  ( 111.4021762516569964, 137.5714195593754710, -35.00000000000000000 ) ) ;
#7456 = CARTESIAN_POINT ( 'NONE',  ( -157.6495955161842062, -161.0130981290893146, 41.15050349809590102 ) ) ;
#7457 = CARTESIAN_POINT ( 'NONE',  ( 46.10157429594899270, 135.8344580088725877, 38.46393386101376421 ) ) ;
#7458 = CARTESIAN_POINT ( 'NONE',  ( 41.64333658814960870, 117.9797705074273182, 38.42115945441014446 ) ) ;
#7459 = CARTESIAN_POINT ( 'NONE',  ( 15.34898554898258460, 114.0222161449793248, 7.937823431466153323 ) ) ;
#7460 = CARTESIAN_POINT ( 'NONE',  ( -142.0420953463935803, -189.5438272943106881, 52.72008163687743831 ) ) ;
#7461 = CARTESIAN_POINT ( 'NONE',  ( 39.42975644700377558, 98.81518717409400665, 31.60846029578754468 ) ) ;
#7462 = CARTESIAN_POINT ( 'NONE',  ( -148.3790856849358306, -162.6630981290892919, 59.16757674456786020 ) ) ;
#7463 = EDGE_LOOP ( 'NONE', ( #6485, #8526, #443, #18927 ) ) ;
#7464 = CARTESIAN_POINT ( 'NONE',  ( 47.05648932407426344, 157.5844580088725877, 31.27175355779120025 ) ) ;
#7465 = EDGE_CURVE ( 'NONE', #7175, #13745, #18832, .T. ) ;
#7466 = CARTESIAN_POINT ( 'NONE',  ( 39.42188022582085694, 153.9507182763122159, -10.27990332573616961 ) ) ;
#7467 = CARTESIAN_POINT ( 'NONE',  ( 62.17156016504299032, 99.21662021101468554, 6.584824431686855384 ) ) ;
#7468 = CARTESIAN_POINT ( 'NONE',  ( 43.01140435219951996, 155.0344580088726048, 29.21067981925357060 ) ) ;
#7469 = VECTOR ( 'NONE', #6764, 1000.000000000000000 ) ;
#7470 = EDGE_CURVE ( 'NONE', #11596, #10804, #14929, .T. ) ;
#7471 = VECTOR ( 'NONE', #19881, 1000.000000000000000 ) ;
#7472 = CARTESIAN_POINT ( 'NONE',  ( 41.64333658814960870, 78.97977050742731819, 38.42115945441014446 ) ) ;
#7473 = EDGE_LOOP ( 'NONE', ( #8482, #10075, #9524, #20401 ) ) ;
#7474 = ADVANCED_FACE ( 'NONE', ( #18620 ), #12100, .F. ) ;
#7475 = VERTEX_POINT ( 'NONE', #15425 ) ;
#7476 = VECTOR ( 'NONE', #17735, 1000.000000000000000 ) ;
#7477 = DIRECTION ( 'NONE',  ( 0.5573926701119623628, -0.8302490056034136368, 0.000000000000000000 ) ) ;
#7478 = ADVANCED_FACE ( 'NONE', ( #20708 ), #13969, .T. ) ;
#7479 = CARTESIAN_POINT ( 'NONE',  ( 46.10157429594899270, 116.6604996726487258, 29.95742577749337343 ) ) ;
#7481 = CARTESIAN_POINT ( 'NONE',  ( 67.48508721674359379, 143.7297851702464015, -1.275552590249036777 ) ) ;
#7480 = CARTESIAN_POINT ( 'NONE',  ( 44.37947211624943833, 82.01518717409400949, 38.42115945441014446 ) ) ;
#7482 = CARTESIAN_POINT ( 'NONE',  ( -157.2955611005345986, -167.3438272943107279, 41.63779006702063867 ) ) ;
#7483 = CARTESIAN_POINT ( 'NONE',  ( 57.67197451322198276, 240.2871645992281628, -6.999999999999982236 ) ) ;
#7484 = CARTESIAN_POINT ( 'NONE',  ( -161.4692556286852607, -187.4130981290893203, 52.90620854394536821 ) ) ;
#7485 = VECTOR ( 'NONE', #2625, 1000.000000000000000 ) ;
#7486 = CARTESIAN_POINT ( 'NONE',  ( 144.5586921005913439, 133.1239846058259388, -35.00000000000000000 ) ) ;
#7487 = CARTESIAN_POINT ( 'NONE',  ( -141.4692556286852891, -162.8391397928654101, 46.40781461928724383 ) ) ;
#7488 = CARTESIAN_POINT ( 'NONE',  ( 41.64333658814960870, 140.7797705074273154, 30.00020018409699318 ) ) ;
#7489 = CARTESIAN_POINT ( 'NONE',  ( 8.867590775667826719, 116.4845415224344833, 7.977433149383395872 ) ) ;
#7490 = CARTESIAN_POINT ( 'NONE',  ( 41.64333658814960870, 138.7151871740940123, 38.42115945441014446 ) ) ;
#7491 = VECTOR ( 'NONE', #19667, 1000.000000000000000 ) ;
#7492 = CARTESIAN_POINT ( 'NONE',  ( 43.80332655382220253, 137.8836182503284533, 29.21067981925356705 ) ) ;
#7493 = CARTESIAN_POINT ( 'NONE',  ( -148.5561028927606344, -163.2584106276440536, 58.62277379824867296 ) ) ;
#7494 = EDGE_CURVE ( 'NONE', #20206, #19334, #17273, .T. ) ;
#7495 = DIRECTION ( 'NONE',  ( 0.000000000000000000, 0.000000000000000000, -1.000000000000000000 ) ) ;
#7496 = DIRECTION ( 'NONE',  ( 0.9387810623359077455, 0.3426822732243072211, 0.03548206049944095664 ) ) ;
#7497 = CARTESIAN_POINT ( 'NONE',  ( 62.38482844916680392, 99.30468409114129713, 12.58043553469319953 ) ) ;
#7498 = FACE_OUTER_BOUND ( 'NONE', #17738, .T. ) ;
#7499 = CARTESIAN_POINT ( 'NONE',  ( 44.37947211624943833, 103.0151871740939953, 38.42115945441014446 ) ) ;
#7500 = ADVANCED_FACE ( 'NONE', ( #8705 ), #3633, .F. ) ;
#7501 = ORIENTED_EDGE ( 'NONE', *, *, #4258, .T. ) ;
#7502 = PLANE ( 'NONE',  #6785 ) ;
#7503 = ORIENTED_EDGE ( 'NONE', *, *, #12229, .F. ) ;
#7504 = CARTESIAN_POINT ( 'NONE',  ( 38.96631938032478359, 90.08445800887257349, 37.14960608071593384 ) ) ;
#7505 = CARTESIAN_POINT ( 'NONE',  ( 39.42975644700377558, 147.6797705074273495, 36.81289934271958941 ) ) ;
#7506 = CARTESIAN_POINT ( 'NONE',  ( 46.10157429594899270, 148.7604996726487627, 38.46393386101376421 ) ) ;
#7508 = CARTESIAN_POINT ( 'NONE',  ( 20.50804704269433998, 103.0453634090187762, -11.55335571609641399 ) ) ;
#7507 = CARTESIAN_POINT ( 'NONE',  ( 46.59305225739526435, 109.3151871740939924, 36.81289934271958941 ) ) ;
#7509 = ADVANCED_FACE ( 'NONE', ( #3524 ), #2306, .T. ) ;
#7510 = CARTESIAN_POINT ( 'NONE',  ( 45.05633291560662457, 59.76197383743925684, 29.61780626570246966 ) ) ;
#7512 = CARTESIAN_POINT ( 'NONE',  ( -141.4692556286852891, -183.0630981290892976, 49.65701158161630957 ) ) ;
#7511 = LINE ( 'NONE', #14210, #17134 ) ;
#7513 = CARTESIAN_POINT ( 'NONE',  ( -151.4692556286852891, -192.8130981290892692, 59.65701158161632378 ) ) ;
#7514 = CARTESIAN_POINT ( 'NONE',  ( -151.4692556286852891, -196.9891397928655010, 59.65701158161632378 ) ) ;
#7515 = CARTESIAN_POINT ( 'NONE',  ( 38.58424406990784661, 66.26518717409400949, 35.64915139335016647 ) ) ;
#7516 = CARTESIAN_POINT ( 'NONE',  ( 46.10157429594899270, 104.6604996726487116, 29.95742577749336988 ) ) ;
#7517 = CARTESIAN_POINT ( 'NONE',  ( -159.0959885057557983, -170.1938272943107222, 44.11586579668791330 ) ) ;
#7518 = CARTESIAN_POINT ( 'NONE',  ( -160.8964159109769696, -194.1584106276440593, 49.65701158161630957 ) ) ;
#7519 = EDGE_LOOP ( 'NONE', ( #4692, #16423, #7420, #12447 ) ) ;
#7520 = CARTESIAN_POINT ( 'NONE',  ( -159.0959885057557983, -178.8584106276440480, 55.19815736654470584 ) ) ;
#7521 = CARTESIAN_POINT ( 'NONE',  ( 30.01547214559559507, 151.6658481390280144, 9.406004577920295873 ) ) ;
#7522 = DIRECTION ( 'NONE',  ( 0.000000000000000000, 0.000000000000000000, 1.000000000000000000 ) ) ;
#7523 = CARTESIAN_POINT ( 'NONE',  ( 47.43856463449118621, 142.6151871740939896, 34.21067981925357060 ) ) ;
#7524 = CARTESIAN_POINT ( 'NONE',  ( 39.42975644700377558, 102.6797705074273210, 36.81289934271958941 ) ) ;
#7525 = EDGE_LOOP ( 'NONE', ( #19852, #1795, #4826, #9641 ) ) ;
#7526 = ORIENTED_EDGE ( 'NONE', *, *, #15389, .F. ) ;
#7527 = CARTESIAN_POINT ( 'NONE',  ( 57.86150831142030171, 95.93494642397840266, -0.2007220744356660869 ) ) ;
#7528 = ORIENTED_EDGE ( 'NONE', *, *, #4813, .T. ) ;
#7529 = CARTESIAN_POINT ( 'NONE',  ( 38.96631938032478359, 114.0844580088725877, 37.14960608071593384 ) ) ;
#7530 = DIRECTION ( 'NONE',  ( 0.000000000000000000, 0.000000000000000000, 1.000000000000000000 ) ) ;
#7531 = CARTESIAN_POINT ( 'NONE',  ( 46.59305225739526435, 80.17977050742732104, 31.60846029578754468 ) ) ;
#7532 = CARTESIAN_POINT ( 'NONE',  ( 44.37947211624943833, 134.2151871740940123, 30.00020018409699318 ) ) ;
#7533 = CARTESIAN_POINT ( 'NONE',  ( 46.10157429594899270, 100.7604996726487485, 38.46393386101376421 ) ) ;
#7534 = CARTESIAN_POINT ( 'NONE',  ( 77.24268685965694203, 120.2105100216710696, 12.57728155048203433 ) ) ;
#7535 = DIRECTION ( 'NONE',  ( 0.000000000000000000, -1.000000000000000000, 0.000000000000000000 ) ) ;
#7536 = CARTESIAN_POINT ( 'NONE',  ( -157.6495955161842062, -164.0391397928654555, 58.16351966513671812 ) ) ;
#7537 =( BOUNDED_CURVE ( )  B_SPLINE_CURVE ( 2, ( #21148, #7492, #20933, #5814, #12545, #7711, #6032, #12762, #4374, #19273, #4174, #10902, #11105 ),
 .UNSPECIFIED., .F., .F. ) 
 B_SPLINE_CURVE_WITH_KNOTS ( ( 3, 2, 2, 2, 2, 2, 3 ),
 ( 0.2132352941176470507, 0.2147058823529411631, 0.2176470588235294157, 0.2205882352941176405, 0.2235294117647058931, 0.2264705882352941180, 0.2279411764705882304 ),
 .UNSPECIFIED. ) 
 CURVE ( )  GEOMETRIC_REPRESENTATION_ITEM ( )  RATIONAL_B_SPLINE_CURVE ( ( 0.9755282581475768211, 0.9755282581475768211, 1.000000000000000000, 0.9510565162951535312, 1.000000000000000000, 0.9510565162951535312, 1.000000000000000000, 0.9510565162951535312, 1.000000000000000000, 0.9510565162951535312, 1.000000000000000000, 0.9755282581475768211, 0.9755282581475768211 ) ) 
 REPRESENTATION_ITEM ( '' )  );
#7538 = DIRECTION ( 'NONE',  ( 0.000000000000000000, 0.000000000000000000, 1.000000000000000000 ) ) ;
#7539 = UNCERTAINTY_MEASURE_WITH_UNIT (LENGTH_MEASURE( 1.000000000000000082E-05 ), #5118, 'distance_accuracy_value', 'NONE');
#7540 = EDGE_CURVE ( 'NONE', #13261, #13667, #15823, .T. ) ;
#7541 = VECTOR ( 'NONE', #19248, 1000.000000000000000 ) ;
#7542 = CARTESIAN_POINT ( 'NONE',  ( -151.4692556286853176, -164.3130981290893260, 39.65701158161629536 ) ) ;
#7543 = EDGE_LOOP ( 'NONE', ( #4627, #9285 ) ) ;
#7544 = CARTESIAN_POINT ( 'NONE',  ( 47.43856463449117200, 85.72977050742731819, 35.64915139335016647 ) ) ;
#7545 = CARTESIAN_POINT ( 'NONE',  ( -143.8425227516148084, -162.0938272943107279, 44.11586579668791330 ) ) ;
#7546 = CARTESIAN_POINT ( 'NONE',  ( 20.75180444880664510, 93.89949152720284076, -5.875022464008872625 ) ) ;
#7547 = CARTESIAN_POINT ( 'NONE',  ( -159.0959885057557983, -190.8584106276440480, 55.19815736654470584 ) ) ;
#7548 = ORIENTED_EDGE ( 'NONE', *, *, #8548, .T. ) ;
#7549 = CARTESIAN_POINT ( 'NONE',  ( -157.6495955161842062, -175.1130981290893089, 58.16351966513671812 ) ) ;
#7550 = AXIS2_PLACEMENT_3D ( 'NONE', #3847, #20601, #19054 ) ;
#7551 = CARTESIAN_POINT ( 'NONE',  ( 39.42975644700377558, 132.6797705074273210, 36.81289934271958941 ) ) ;
#7552 = CARTESIAN_POINT ( 'NONE',  ( 23.54274795406405474, 91.84646939011692268, -11.98975411606233976 ) ) ;
#7553 = VERTEX_POINT ( 'NONE', #1980 ) ;
#7554 = CARTESIAN_POINT ( 'NONE',  ( 156.7804311855217065, 208.8003142469820830, -29.99999999999997868 ) ) ;
#7555 = VERTEX_POINT ( 'NONE', #8822 ) ;
#7556 = CARTESIAN_POINT ( 'NONE',  ( 38.58424406990784661, 129.2297705074273324, 32.77220824515698183 ) ) ;
#7557 = ADVANCED_FACE ( 'NONE', ( #10685 ), #8713, .T. ) ;
#7558 = CARTESIAN_POINT ( 'NONE',  ( 44.55648932407425633, 109.6104996726487428, 38.96596240072933170 ) ) ;
#7559 = LINE ( 'NONE', #14049, #7993 ) ;
#7560 = CARTESIAN_POINT ( 'NONE',  ( 42.21948215057684450, 129.0373810949690210, 29.21067981925356705 ) ) ;
#7561 = SURFACE_STYLE_USAGE ( .BOTH. , #17460 ) ;
#7562 = CARTESIAN_POINT ( 'NONE',  ( -148.5561028927606344, -159.0584106276440650, 40.69124936498395328 ) ) ;
#7563 = CARTESIAN_POINT ( 'NONE',  ( 38.58424406990786082, 99.11518717409400381, 34.21067981925357060 ) ) ;
#7564 = CARTESIAN_POINT ( 'NONE',  ( 43.01140435219954838, 132.5344580088725763, 39.21067981925356349 ) ) ;
#7565 = CARTESIAN_POINT ( 'NONE',  ( 136.0032066456581390, 182.5367998656340944, 34.00000000000001421 ) ) ;
#7566 = CARTESIAN_POINT ( 'NONE',  ( -145.2889157411863721, -161.6130981290892805, 41.15050349809590102 ) ) ;
#7567 = CARTESIAN_POINT ( 'NONE',  ( 38.96631938032478359, 132.0844580088725877, 37.14960608071593384 ) ) ;
#7568 = CARTESIAN_POINT ( 'NONE',  ( 48.01140435219951996, 133.4344580088725820, 32.58608133808903773 ) ) ;
#7569 = CARTESIAN_POINT ( 'NONE',  ( 39.42975644700377558, 117.6797705074273210, 36.81289934271958941 ) ) ;
#7570 = CARTESIAN_POINT ( 'NONE',  ( 32.24825037804825456, 146.0601464669000791, 9.485560667832931614 ) ) ;
#7571 = CARTESIAN_POINT ( 'NONE',  ( -142.0420953463936087, -189.3938272943107393, 49.65701158161630957 ) ) ;
#7572 = CARTESIAN_POINT ( 'NONE',  ( 38.58424406990785371, 98.96518717409398391, 32.77220824515697473 ) ) ;
#7573 = CARTESIAN_POINT ( 'NONE',  ( 38.01140435219952707, 90.86049967264872862, 35.83527830041809636 ) ) ;
#7574 = VERTEX_POINT ( 'NONE', #5392 ) ;
#7575 = LINE ( 'NONE', #14275, #12948 ) ;
#7576 = EDGE_CURVE ( 'NONE', #19802, #393, #18076, .T. ) ;
#7577 = CARTESIAN_POINT ( 'NONE',  ( 9.021810916323596885, 123.9851095102452945, 2.220310480865780534 ) ) ;
#7578 = CARTESIAN_POINT ( 'NONE',  ( 58.43892221570314405, 143.5117748958429047, 4.561220828673259398 ) ) ;
#7579 = CARTESIAN_POINT ( 'NONE',  ( 44.55648932407425633, 154.8844580088725991, 29.45539723777780239 ) ) ;
#7580 = CARTESIAN_POINT ( 'NONE',  ( 39.42975644700377558, 75.67977050742732104, 36.81289934271958941 ) ) ;
#7581 = ORIENTED_EDGE ( 'NONE', *, *, #3602, .T. ) ;
#7582 = ORIENTED_EDGE ( 'NONE', *, *, #20163, .T. ) ;
#7583 = CARTESIAN_POINT ( 'NONE',  ( 40.27526882409969033, 155.9297705074273210, 30.44471234641811819 ) ) ;
#7584 = CARTESIAN_POINT ( 'NONE',  ( -141.4692556286852891, -164.9130981290892919, 46.40781461928724383 ) ) ;
#7585 = AXIS2_PLACEMENT_3D ( 'NONE', #12636, #19357, #4255 ) ;
#7587 = EDGE_CURVE ( 'NONE', #20193, #11386, #16959, .T. ) ;
#7586 = CARTESIAN_POINT ( 'NONE',  ( 44.55648932407425633, 119.8104996726487457, 29.45539723777780239 ) ) ;
#7589 = CARTESIAN_POINT ( 'NONE',  ( 48.37701604703377001, 153.6359454806530778, -1.989754116034292197 ) ) ;
#7588 = CARTESIAN_POINT ( 'NONE',  ( 47.43856463449117200, 73.46518717409398391, 35.64915139335016647 ) ) ;
#7590 = ADVANCED_FACE ( 'NONE', ( #7058, #15631, #328 ), #437, .T. ) ;
#7591 = CARTESIAN_POINT ( 'NONE',  ( -154.3824083646099439, -169.2938272943107165, 58.62277379824867296 ) ) ;
#7592 = CARTESIAN_POINT ( 'NONE',  ( 23.42018083028975184, 147.9700754799198705, 17.16443675223517573 ) ) ;
#7593 = CARTESIAN_POINT ( 'NONE',  ( -148.3790856849358306, -183.6630981290893203, 59.16757674456786020 ) ) ;
#7594 = CARTESIAN_POINT ( 'NONE',  ( 43.01140435219951286, 62.96049967264873004, 29.21067981925356705 ) ) ;
#7595 = CARTESIAN_POINT ( 'NONE',  ( 46.10157429594899270, 156.8344580088725309, 38.46393386101376421 ) ) ;
#7596 = CARTESIAN_POINT ( 'NONE',  ( 43.01140435219951286, 142.1297705074273097, 38.86567161673127657 ) ) ;
#7597 = ADVANCED_FACE ( 'NONE', ( #7167 ), #13870, .T. ) ;
#7598 = CARTESIAN_POINT ( 'NONE',  ( 15.20278999188385960, 140.0102622722330636, 1.787054806504753346 ) ) ;
#7599 = CARTESIAN_POINT ( 'NONE',  ( 40.27526882409969744, 123.5651871740939924, 37.97664729208901235 ) ) ;
#7600 = CARTESIAN_POINT ( 'NONE',  ( -155.3247660971250923, -155.7098880568450454, 40.99743995317548695 ) ) ;
#7601 = CARTESIAN_POINT ( 'NONE',  ( 40.27526882409969033, 60.82977050742731961, 37.97664729208901946 ) ) ;
#7602 = CARTESIAN_POINT ( 'NONE',  ( 5.130598475945862827E-15, 0.000000000000000000, 5.000000000000018652 ) ) ;
#7603 = CARTESIAN_POINT ( 'NONE',  ( 15.94687047784549172, 111.7036002239776451, 14.84254118869207417 ) ) ;
#7604 = CIRCLE ( 'NONE', #9361, 15.54735917280169311 ) ;
#7605 = CARTESIAN_POINT ( 'NONE',  ( 38.01140435219952707, 120.8604996726487428, 35.83527830041809636 ) ) ;
#7606 = CARTESIAN_POINT ( 'NONE',  ( 44.37947211624943833, 110.2151871740940123, 30.00020018409699318 ) ) ;
#7607 = ORIENTED_EDGE ( 'NONE', *, *, #10183, .T. ) ;
#7608 = CARTESIAN_POINT ( 'NONE',  ( 141.1725454929228079, -61.68114226949890622, 10.00000000000001599 ) ) ;
#7609 = VERTEX_POINT ( 'NONE', #21362 ) ;
#7610 = CARTESIAN_POINT ( 'NONE',  ( 38.01140435219951996, 89.63445800887258486, 32.58608133808903773 ) ) ;
#7611 = CARTESIAN_POINT ( 'NONE',  ( 38.01140435219952707, 159.7104996726487514, 34.21067981925357060 ) ) ;
#7612 = VECTOR ( 'NONE', #3396, 1000.000000000000227 ) ;
#7613 = CARTESIAN_POINT ( 'NONE',  ( 44.55648932407425633, 146.8104996726487457, 29.45539723777780239 ) ) ;
#7615 = CARTESIAN_POINT ( 'NONE',  ( 58.57598713290192904, 143.3259681031794059, -1.434385245616870197 ) ) ;
#7614 = CARTESIAN_POINT ( 'NONE',  ( 44.37947211624943833, 106.0151871740939953, 38.42115945441014446 ) ) ;
#7616 = AXIS2_PLACEMENT_3D ( 'NONE', #2144, #8877, #15584 ) ;
#7617 = DIRECTION ( 'NONE',  ( -0.000000000000000000, -0.000000000000000000, 1.000000000000000000 ) ) ;
#7619 = CARTESIAN_POINT ( 'NONE',  ( -143.3790856849358306, -182.7630981290893146, 43.77915905869157598 ) ) ;
#7618 = CARTESIAN_POINT ( 'NONE',  ( 48.01123829699398726, 144.4020089423098341, 33.87806037135994330 ) ) ;
#7620 = CARTESIAN_POINT ( 'NONE',  ( 46.10157429594899270, 118.7344580088725650, 29.95742577749336988 ) ) ;
#7621 = VECTOR ( 'NONE', #1031, 1000.000000000000000 ) ;
#7622 = CYLINDRICAL_SURFACE ( 'NONE', #7907, 10.00000000000000888 ) ;
#7623 = DIRECTION ( 'NONE',  ( -0.000000000000000000, -0.000000000000000000, -1.000000000000000000 ) ) ;
#7624 = CARTESIAN_POINT ( 'NONE',  ( 46.59305225739526435, 70.91518717409398675, 31.60846029578754468 ) ) ;
#7625 = CARTESIAN_POINT ( 'NONE',  ( 28.88048086162541850, 151.0887240815949895, -10.63664014359656385 ) ) ;
#7626 = CARTESIAN_POINT ( 'NONE',  ( 47.05648932407426344, 94.91049967264873999, 37.14960608071593384 ) ) ;
#7627 = CARTESIAN_POINT ( 'NONE',  ( -142.0420953463936087, -174.3938272943107393, 49.65701158161630957 ) ) ;
#7628 = FACE_OUTER_BOUND ( 'NONE', #10986, .T. ) ;
#7629 = ORIENTED_EDGE ( 'NONE', *, *, #10210, .F. ) ;
#7630 = CARTESIAN_POINT ( 'NONE',  ( 71.48324150724619130, 139.0594858779678873, 3.930207297951037848 ) ) ;
#7631 = DIRECTION ( 'NONE',  ( 0.000000000000000000, -1.000000000000000000, 0.000000000000000000 ) ) ;
#7632 = CARTESIAN_POINT ( 'NONE',  ( 38.58424406990784661, 138.2651871740939669, 35.64915139335016647 ) ) ;
#7633 = CARTESIAN_POINT ( 'NONE',  ( 39.42975644700377558, 156.4151871740940010, 36.81289934271958941 ) ) ;
#7634 = CARTESIAN_POINT ( 'NONE',  ( 39.42975644700377558, 96.67977050742732104, 36.81289934271958941 ) ) ;
#7635 = VECTOR ( 'NONE', #11021, 1000.000000000000000 ) ;
#7636 = ORIENTED_EDGE ( 'NONE', *, *, #1349, .F. ) ;
#7637 = ORIENTED_EDGE ( 'NONE', *, *, #6001, .F. ) ;
#7638 = AXIS2_PLACEMENT_3D ( 'NONE', #19275, #10905, #17608 ) ;
#7639 = CARTESIAN_POINT ( 'NONE',  ( 15.18239976710701100, 124.4615124019231018, 16.34704286353642999 ) ) ;
#7640 = AXIS2_PLACEMENT_3D ( 'NONE', #2655, #11037, #4747 ) ;
#7641 = VERTEX_POINT ( 'NONE', #1187 ) ;
#7642 = CARTESIAN_POINT ( 'NONE',  ( 41.46631938032478359, 113.1844580088725820, 29.45539723777780239 ) ) ;
#7643 = CARTESIAN_POINT ( 'NONE',  ( 42.21948215057684450, 75.03738109496899256, 29.21067981925356705 ) ) ;
#7644 = EDGE_CURVE ( 'NONE', #9069, #9746, #3333, .T. ) ;
#7645 = ADVANCED_FACE ( 'NONE', ( #21259 ), #15952, .F. ) ;
#7646 = CARTESIAN_POINT ( 'NONE',  ( 40.27526882409969033, 80.92977050742729261, 30.44471234641811819 ) ) ;
#7647 = CARTESIAN_POINT ( 'NONE',  ( 40.27526882409969033, 131.6651871740939725, 30.44471234641811819 ) ) ;
#7648 = MANIFOLD_SOLID_BREP ( 'Boss-Extrude14', #8831 ) ;
#7649 = CARTESIAN_POINT ( 'NONE',  ( 44.55648932407425633, 91.61049967264874283, 38.96596240072933170 ) ) ;
#7650 = CARTESIAN_POINT ( 'NONE',  ( 24.41145734808947054, 148.6458414325078081, 10.19629000755267434 ) ) ;
#7651 = CARTESIAN_POINT ( 'NONE',  ( 39.35878039893513858, 95.17507832528838208, 37.62897400776943613 ) ) ;
#7652 = CARTESIAN_POINT ( 'NONE',  ( -154.5594255724347761, -165.0891397928654669, 40.14644641866476604 ) ) ;
#7653 = VECTOR ( 'NONE', #14968, 1000.000000000000000 ) ;
#7654 = CARTESIAN_POINT ( 'NONE',  ( 43.01140435219951996, 153.5344580088726048, 39.21067981925357060 ) ) ;
#7655 = CARTESIAN_POINT ( 'NONE',  ( 157.5268905834513475, 193.0332408774651185, -19.99999999999997868 ) ) ;
#7656 = PRODUCT_DEFINITION_SHAPE ( 'NONE', 'NONE',  #21828 ) ;
#7657 = CARTESIAN_POINT ( 'NONE',  ( 43.80332655382220253, 106.9575765865522925, 29.21067981925356705 ) ) ;
#7658 = VERTEX_POINT ( 'NONE', #14193 ) ;
#7659 = CARTESIAN_POINT ( 'NONE',  ( 47.43856463449118621, 79.87977050742732388, 34.21067981925357060 ) ) ;
#7660 = CARTESIAN_POINT ( 'NONE',  ( -142.0420953463935803, -165.5438272943107165, 52.72008163687743831 ) ) ;
#7661 = CARTESIAN_POINT ( 'NONE',  ( 18.86674891209846905, 143.9013856721611546, -11.04182128657428485 ) ) ;
#7662 = CARTESIAN_POINT ( 'NONE',  ( -160.8964159109769696, -194.3084106276440366, 46.59394152635518793 ) ) ;
#7663 = ORIENTED_EDGE ( 'NONE', *, *, #21455, .T. ) ;
#7664 = DIRECTION ( 'NONE',  ( 0.000000000000000000, 0.000000000000000000, 1.000000000000000000 ) ) ;
#7665 = CARTESIAN_POINT ( 'NONE',  ( 47.05648932407426344, 124.5844580088725735, 31.27175355779120025 ) ) ;
#7666 = CARTESIAN_POINT ( 'NONE',  ( 44.37947211624943833, 127.2797705074273438, 38.42115945441014446 ) ) ;
#7667 = AXIS2_PLACEMENT_3D ( 'NONE', #17117, #160, #5435 ) ;
#7668 = ORIENTED_EDGE ( 'NONE', *, *, #6572, .T. ) ;
#7669 = LINE ( 'NONE', #17347, #3423 ) ;
#7670 = ORIENTED_EDGE ( 'NONE', *, *, #9283, .F. ) ;
#7671 = CARTESIAN_POINT ( 'NONE',  ( 47.43856463449117200, 127.7297705074272898, 35.64915139335016647 ) ) ;
#7672 = CARTESIAN_POINT ( 'NONE',  ( 44.55648932407425633, 134.8104996726487457, 29.45539723777780239 ) ) ;
#7673 = EDGE_CURVE ( 'NONE', #17454, #5192, #20351, .T. ) ;
#7674 =( BOUNDED_CURVE ( )  B_SPLINE_CURVE ( 2, ( #8239, #12971, #14941, #9566, #21688, #13304, #2826, #6466, #4809, #11531, #1398, #20042, #14509 ),
 .UNSPECIFIED., .F., .T. ) 
 B_SPLINE_CURVE_WITH_KNOTS ( ( 3, 2, 2, 2, 2, 2, 3 ),
 ( 0.6102941176470587648, 0.6117647058823529882, 0.6147058823529412130, 0.6176470588235294379, 0.6205882352941176627, 0.6235294117647058876, 0.6250000000000000000 ),
 .UNSPECIFIED. ) 
 CURVE ( )  GEOMETRIC_REPRESENTATION_ITEM ( )  RATIONAL_B_SPLINE_CURVE ( ( 0.9755282581475768211, 0.9755282581475758219, 1.000000000000000000, 0.9510565162951535312, 1.000000000000000000, 0.9510565162951535312, 1.000000000000000000, 0.9510565162951535312, 1.000000000000000000, 0.9510565162951535312, 1.000000000000000000, 0.9755282581475768211, 0.9755282581475768211 ) ) 
 REPRESENTATION_ITEM ( '' )  );
#7675 = CARTESIAN_POINT ( 'NONE',  ( 42.21948215057684450, 99.03738109496899256, 29.21067981925356705 ) ) ;
#7676 = CARTESIAN_POINT ( 'NONE',  ( 38.01140435219952707, 129.5604996726487457, 32.58608133808903773 ) ) ;
#7677 = CARTESIAN_POINT ( 'NONE',  ( -154.5594255724347761, -193.8891397928654783, 59.16757674456785310 ) ) ;
#7678 = VECTOR ( 'NONE', #15407, 1000.000000000000114 ) ;
#7679 = CARTESIAN_POINT ( 'NONE',  ( 83.67254549292280785, -61.68114226949890622, -46.21320343559645494 ) ) ;
#7680 = LINE ( 'NONE', #19027, #15673 ) ;
#7681 = CARTESIAN_POINT ( 'NONE',  ( -161.4692556286852607, -160.4130981290893203, 52.90620854394536821 ) ) ;
#7682 = SHAPE_DEFINITION_REPRESENTATION ( #6046, #3970 ) ;
#7683 = CARTESIAN_POINT ( 'NONE',  ( 47.05648932407426344, 135.9844580088725934, 37.14960608071593384 ) ) ;
#7684 = CARTESIAN_POINT ( 'NONE',  ( 39.42975644700377558, 108.6797705074273352, 36.81289934271958941 ) ) ;
#7685 = CARTESIAN_POINT ( 'NONE',  ( 17.21810733192966936, 108.3100148859214329, 7.699684045823485867 ) ) ;
#7686 = CARTESIAN_POINT ( 'NONE',  ( -157.2955611005346270, -193.4438272943106938, 57.67623309621198047 ) ) ;
#7687 = CARTESIAN_POINT ( 'NONE',  ( 40.27526882409969744, 99.56518717409400665, 37.97664729208901235 ) ) ;
#7688 = AXIS2_PLACEMENT_3D ( 'NONE', #9651, #16352, #6680 ) ;
#7689 = CARTESIAN_POINT ( 'NONE',  ( -145.2889157411863437, -161.6130981290892805, 41.15050349809589392 ) ) ;
#7690 = VERTEX_POINT ( 'NONE', #12438 ) ;
#7691 = CARTESIAN_POINT ( 'NONE',  ( -151.4692556286853176, -165.2391397928654442, 39.65701158161629536 ) ) ;
#7692 = CARTESIAN_POINT ( 'NONE',  ( 77.19215121279506775, 118.0176990621192203, -1.351406188750652992 ) ) ;
#7693 = CARTESIAN_POINT ( 'NONE',  ( 15.53781593631592983, 113.9137188375014347, -11.07707013084618097 ) ) ;
#7694 = CARTESIAN_POINT ( 'NONE',  ( 43.01140435219951996, 153.5344580088726048, 39.21067981925357060 ) ) ;
#7695 = CARTESIAN_POINT ( 'NONE',  ( 38.58424406990785371, 78.52977050742730114, 35.64915139335015937 ) ) ;
#7696 = EDGE_LOOP ( 'NONE', ( #13669, #14567, #6669, #1959 ) ) ;
#7697 = ORIENTED_EDGE ( 'NONE', *, *, #3159, .F. ) ;
#7698 = CARTESIAN_POINT ( 'NONE',  ( 38.58424406990784661, 153.5297705074273154, 35.64915139335016647 ) ) ;
#7699 = DIRECTION ( 'NONE',  ( -1.000000000000000000, 0.000000000000000000, 1.915514545828640705E-16 ) ) ;
#7700 = CARTESIAN_POINT ( 'NONE',  ( 39.92123440845004723, 124.1604996726487400, 38.46393386101376421 ) ) ;
#7702 = CARTESIAN_POINT ( 'NONE',  ( 72.81290617574171620, 103.2231620977376281, 0.1530188383368442095 ) ) ;
#7701 = CARTESIAN_POINT ( 'NONE',  ( 46.59305225739526435, 79.31518717409399244, 36.81289934271958941 ) ) ;
#7703 = CARTESIAN_POINT ( 'NONE',  ( -159.0959885057557983, -167.1938272943107222, 44.11586579668791330 ) ) ;
#7704 = CARTESIAN_POINT ( 'NONE',  ( 43.80332655382220253, 112.5373810949689926, 39.21067981925355639 ) ) ;
#7705 = CARTESIAN_POINT ( 'NONE',  ( -161.4692556286853176, -187.5630981290892976, 49.65701158161630957 ) ) ;
#7706 = DIRECTION ( 'NONE',  ( 1.723963091245776585E-16, 6.336983651701954299E-17, 1.000000000000000000 ) ) ;
#7707 = CARTESIAN_POINT ( 'NONE',  ( -143.3790856849358306, -163.2891397928654555, 55.53486410454105027 ) ) ;
#7708 = CARTESIAN_POINT ( 'NONE',  ( 38.58424406990786082, 141.3797705074273381, 34.21067981925357060 ) ) ;
#7709 = CARTESIAN_POINT ( 'NONE',  ( 47.52490801233957995, 85.89149910694642642, 6.191896081848653921 ) ) ;
#7710 = CARTESIAN_POINT ( 'NONE',  ( 43.01140435219951286, 126.8651871740939896, 38.86567161673127657 ) ) ;
#7711 = CARTESIAN_POINT ( 'NONE',  ( 48.01140435219951996, 137.3604996726487286, 32.58608133808903773 ) ) ;
#7712 = DIRECTION ( 'NONE',  ( 1.387778780781445676E-16, 1.000000000000000000, 0.000000000000000000 ) ) ;
#7713 = ADVANCED_FACE ( 'NONE', ( #19590 ), #4064, .T. ) ;
#7714 = DIRECTION ( 'NONE',  ( 0.000000000000000000, 0.000000000000000000, 1.000000000000000000 ) ) ;
#7715 = CARTESIAN_POINT ( 'NONE',  ( 68.93731127356984700, 108.6095829621005180, 19.12825547442421126 ) ) ;
#7716 =( NAMED_UNIT ( * ) SI_UNIT ( $, .STERADIAN. ) SOLID_ANGLE_UNIT ( ) );
#7717 = CARTESIAN_POINT ( 'NONE',  ( 41.64333658814960870, 105.7151871740940123, 38.42115945441014446 ) ) ;
#7718 = ORIENTED_EDGE ( 'NONE', *, *, #8167, .T. ) ;
#7719 = CARTESIAN_POINT ( 'NONE',  ( -151.4692556286852607, -156.2391397928654726, 39.65701158161629536 ) ) ;
#7720 = EDGE_LOOP ( 'NONE', ( #6291, #20740, #16315, #20191 ) ) ;
#7721 = CARTESIAN_POINT ( 'NONE',  ( 38.01140435219952707, 95.78445800887259054, 34.21067981925357060 ) ) ;
#7722 = CARTESIAN_POINT ( 'NONE',  ( 47.05648932407426344, 102.9844580088725792, 37.14960608071593384 ) ) ;
#7723 = CARTESIAN_POINT ( 'NONE',  ( 38.01140435219952707, 147.7104996726487514, 34.21067981925357060 ) ) ;
#7725 = CARTESIAN_POINT ( 'NONE',  ( 46.34060549886174840, 91.98545359010019240, -5.720099531362743406 ) ) ;
#7724 = CARTESIAN_POINT ( 'NONE',  ( 47.43856463449117200, 109.4651871740940123, 35.64915139335016647 ) ) ;
#7726 = CARTESIAN_POINT ( 'NONE',  ( 48.01140435219951996, 65.06049967264873146, 35.83527830041810347 ) ) ;
#7728 = CARTESIAN_POINT ( 'NONE',  ( -157.6495955161842062, -157.1130981290892805, 58.16351966513671812 ) ) ;
#7727 = CARTESIAN_POINT ( 'NONE',  ( 43.01140435219951286, 64.46049967264873715, 39.21067981925356349 ) ) ;
#7729 = VECTOR ( 'NONE', #11410, 1000.000000000000000 ) ;
#7730 = CARTESIAN_POINT ( 'NONE',  ( -159.5594255724347761, -187.2630981290893146, 55.53486410454104316 ) ) ;
#7731 = CARTESIAN_POINT ( 'NONE',  ( -151.4692556286852891, -196.9891397928655010, 58.65701158161631668 ) ) ;
#7732 =( BOUNDED_CURVE ( )  B_SPLINE_CURVE ( 2, ( #3295, #21707, #6936, #13536, #3625, #13748, #8587, #3517, #10347, #8261, #1529, #17052, #18502 ),
 .UNSPECIFIED., .F., .F. ) 
 B_SPLINE_CURVE_WITH_KNOTS ( ( 3, 2, 2, 2, 2, 2, 3 ),
 ( 0.6985294117647058432, 0.6999999999999999556, 0.7029411764705881804, 0.7058823529411765163, 0.7088235294117647411, 0.7117647058823529660, 0.7132352941176470784 ),
 .UNSPECIFIED. ) 
 CURVE ( )  GEOMETRIC_REPRESENTATION_ITEM ( )  RATIONAL_B_SPLINE_CURVE ( ( 0.9755282581475768211, 0.9755282581475768211, 1.000000000000000000, 0.9510565162951535312, 1.000000000000000000, 0.9510565162951535312, 1.000000000000000000, 0.9510565162951535312, 1.000000000000000000, 0.9510565162951535312, 1.000000000000000000, 0.9755282581475768211, 0.9755282581475768211 ) ) 
 REPRESENTATION_ITEM ( '' )  );
#7733 = CARTESIAN_POINT ( 'NONE',  ( 39.42975644700377558, 71.81518717409400665, 31.60846029578754468 ) ) ;
#7734 = CARTESIAN_POINT ( 'NONE',  ( 32.98198692859195802, 152.6383102900375093, -3.493975233523312962 ) ) ;
#7735 = CARTESIAN_POINT ( 'NONE',  ( 42.21948215057684450, 114.0373810949690210, 29.21067981925356705 ) ) ;
#7736 = CARTESIAN_POINT ( 'NONE',  ( -160.8964159109769696, -167.0438272943106881, 46.59394152635518793 ) ) ;
#7737 = CARTESIAN_POINT ( 'NONE',  ( -148.5561028927606344, -187.2584106276440536, 58.62277379824867296 ) ) ;
#7738 = ORIENTED_EDGE ( 'NONE', *, *, #9514, .T. ) ;
#7739 = CARTESIAN_POINT ( 'NONE',  ( -148.5561028927606344, -171.0584106276440366, 40.69124936498395328 ) ) ;
#7740 = CARTESIAN_POINT ( 'NONE',  ( 52.27439898384277939, 152.9467924839493946, 17.14431721725165758 ) ) ;
#7741 = FACE_OUTER_BOUND ( 'NONE', #15729, .T. ) ;
#7742 = CARTESIAN_POINT ( 'NONE',  ( 47.43856463449117200, 130.4651871740939839, 35.64915139335016647 ) ) ;
#7743 = CARTESIAN_POINT ( 'NONE',  ( 44.37947211624943833, 157.0151871740940237, 38.42115945441014446 ) ) ;
#7744 = CARTESIAN_POINT ( 'NONE',  ( 43.01140435219951286, 92.62977050742732388, 29.55568802177586107 ) ) ;
#7745 = ORIENTED_EDGE ( 'NONE', *, *, #16946, .T. ) ;
#7746 = VERTEX_POINT ( 'NONE', #16059 ) ;
#7747 = VECTOR ( 'NONE', #17136, 1000.000000000000000 ) ;
#7748 = EDGE_CURVE ( 'NONE', #13985, #11079, #7537, .T. ) ;
#7749 = CARTESIAN_POINT ( 'NONE',  ( 70.51576897149806200, 126.1317638695992116, 12.41827883020830470 ) ) ;
#7750 = ORIENTED_EDGE ( 'NONE', *, *, #6906, .F. ) ;
#7751 = EDGE_CURVE ( 'NONE', #13378, #4603, #16490, .T. ) ;
#7752 = DIRECTION ( 'NONE',  ( 0.000000000000000000, 0.000000000000000000, -1.000000000000000000 ) ) ;
#7753 = CARTESIAN_POINT ( 'NONE',  ( 38.58424406990784661, 75.52977050742732956, 35.64915139335016647 ) ) ;
#7754 = CARTESIAN_POINT ( 'NONE',  ( 44.37947211624943833, 131.2151871740940123, 30.00020018409699318 ) ) ;
#7755 = CARTESIAN_POINT ( 'NONE',  ( 48.01140435219951996, 89.21049967264873715, 34.21067981925357060 ) ) ;
#7756 = CARTESIAN_POINT ( 'NONE',  ( 42.68022887774371554, 94.90707761860559799, 39.21067981925356349 ) ) ;
#7757 = CARTESIAN_POINT ( 'NONE',  ( -151.4692556286852891, -156.2391397928654442, 39.14238933923362396 ) ) ;
#7758 = UNCERTAINTY_MEASURE_WITH_UNIT (LENGTH_MEASURE( 1.000000000000000082E-05 ), #10548, 'distance_accuracy_value', 'NONE');
#7759 = DIRECTION ( 'NONE',  ( 1.000000000000000000, 0.000000000000000000, -1.257660470541341077E-16 ) ) ;
#7760 = CARTESIAN_POINT ( 'NONE',  ( 48.01140435219951996, 62.21049967264874425, 34.21067981925357060 ) ) ;
#7761 = AXIS2_PLACEMENT_3D ( 'NONE', #3820, #15711, #406 ) ;
#7762 = ORIENTED_EDGE ( 'NONE', *, *, #6462, .T. ) ;
#7763 = CARTESIAN_POINT ( 'NONE',  ( 43.01140435219951286, 79.12977050742732388, 38.86567161673127657 ) ) ;
#7764 = CARTESIAN_POINT ( 'NONE',  ( -154.3824083646099439, -194.7584106276440536, 40.69124936498395328 ) ) ;
#7765 = CARTESIAN_POINT ( 'NONE',  ( 63.55746018358933469, 147.2895578332197033, -9.446739241148069510 ) ) ;
#7766 = DIRECTION ( 'NONE',  ( 0.000000000000000000, 0.000000000000000000, 1.000000000000000000 ) ) ;
#7767 = ORIENTED_EDGE ( 'NONE', *, *, #20655, .F. ) ;
#7768 = EDGE_CURVE ( 'NONE', #3989, #6015, #16827, .T. ) ;
#7769 = DIRECTION ( 'NONE',  ( -0.000000000000000000, -0.000000000000000000, 1.000000000000000000 ) ) ;
#7770 = DIRECTION ( 'NONE',  ( -0.5061580162706792452, -0.8624407588727069918, 0.000000000000000000 ) ) ;
#7771 = CARTESIAN_POINT ( 'NONE',  ( 45.74753988029934249, 128.3297705074273267, 30.44471234641812174 ) ) ;
#7772 = ORIENTED_EDGE ( 'NONE', *, *, #20824, .T. ) ;
#7773 = ORIENTED_EDGE ( 'NONE', *, *, #8895, .F. ) ;
#7774 = CARTESIAN_POINT ( 'NONE',  ( 43.01140435219951286, 130.1297705074273381, 38.86567161673127657 ) ) ;
#7775 = CARTESIAN_POINT ( 'NONE',  ( -136.6255475934131596, 760.1741454933652449, -3.999999999999980904 ) ) ;
#7776 = CARTESIAN_POINT ( 'NONE',  ( 41.46631938032478359, 63.38445800887257064, 38.96596240072933170 ) ) ;
#7777 = CARTESIAN_POINT ( 'NONE',  ( 111.4021762516569964, 137.5714195593754710, 14.00000000000001776 ) ) ;
#7778 = FACE_OUTER_BOUND ( 'NONE', #9885, .T. ) ;
#7779 = DIRECTION ( 'NONE',  ( 1.000000000000000000, 0.000000000000000000, 0.000000000000000000 ) ) ;
#7780 = CARTESIAN_POINT ( 'NONE',  ( -157.6495955161842062, -185.9391397928654897, 41.15050349809590102 ) ) ;
#7781 = CARTESIAN_POINT ( 'NONE',  ( 43.01140435219951286, 73.46049967264872294, 39.21067981925356349 ) ) ;
#7782 = CARTESIAN_POINT ( 'NONE',  ( 132.5383153295133809, 192.0288997050666921, 21.73429951086134082 ) ) ;
#7783 = CARTESIAN_POINT ( 'NONE',  ( -151.4692556286852891, -191.6438272943107108, 39.74470866294723947 ) ) ;
#7784 = CARTESIAN_POINT ( 'NONE',  ( 39.92123440845004723, 132.2344580088725650, 38.46393386101376421 ) ) ;
#7785 = CARTESIAN_POINT ( 'NONE',  ( 45.74753988029933538, 101.3297705074273267, 30.44471234641811819 ) ) ;
#7786 = CARTESIAN_POINT ( 'NONE',  ( 46.46425003030392986, 147.9761360841216344, 3.056716434341200106 ) ) ;
#7787 = CARTESIAN_POINT ( 'NONE',  ( -151.4692556286852891, -194.6438272943107393, 39.74470866294723947 ) ) ;
#7788 = CARTESIAN_POINT ( 'NONE',  ( 46.59305225739526435, 97.91518717409400097, 31.60846029578754468 ) ) ;
#7789 = DIRECTION ( 'NONE',  ( 0.000000000000000000, 0.000000000000000000, 1.000000000000000000 ) ) ;
#7790 = ORIENTED_EDGE ( 'NONE', *, *, #9681, .F. ) ;
#7791 = DIRECTION ( 'NONE',  ( 0.000000000000000000, 1.000000000000000000, 0.000000000000000000 ) ) ;
#7792 = CARTESIAN_POINT ( 'NONE',  ( 36.55618291757107841, 153.5264344809625641, -3.375052104409746789 ) ) ;
#7793 = CARTESIAN_POINT ( 'NONE',  ( 46.87248680087107999, 147.7605717807558676, -8.934501345478663481 ) ) ;
#7794 = CARTESIAN_POINT ( 'NONE',  ( 71.86557814238962294, 101.4853659568252766, -7.779689512009451136 ) ) ;
#7795 = CARTESIAN_POINT ( 'NONE',  ( 46.59305225739526435, 71.17977050742730682, 31.60846029578754468 ) ) ;
#7796 = ORIENTED_EDGE ( 'NONE', *, *, #12774, .F. ) ;
#7797 = ORIENTED_EDGE ( 'NONE', *, *, #21316, .T. ) ;
#7798 = CARTESIAN_POINT ( 'NONE',  ( 41.64333658814960870, 150.9797705074273324, 38.42115945441014446 ) ) ;
#7799 = CARTESIAN_POINT ( 'NONE',  ( -151.4692556286852891, -194.3130981290893260, 39.65701158161630246 ) ) ;
#7800 = CARTESIAN_POINT ( 'NONE',  ( 47.05648932407426344, 119.5104996726487343, 31.27175355779120025 ) ) ;
#7802 = CARTESIAN_POINT ( 'NONE',  ( 11.23391594879739941, 132.3357020601377769, 10.49983985543964415 ) ) ;
#7801 = CARTESIAN_POINT ( 'NONE',  ( 41.64333658814960870, 75.71518717409401233, 38.42115945441014446 ) ) ;
#7803 = LINE ( 'NONE', #9460, #13448 ) ;
#7804 = CARTESIAN_POINT ( 'NONE',  ( -159.0959885057557983, -176.1938272943107506, 44.11586579668791330 ) ) ;
#7805 = CARTESIAN_POINT ( 'NONE',  ( 53.04203944364535772, 87.17698241397053494, 14.00585298808814194 ) ) ;
#7806 = CARTESIAN_POINT ( 'NONE',  ( -143.3790856849358306, -191.7630981290893146, 43.77915905869157598 ) ) ;
#7807 = SHAPE_REPRESENTATION_RELATIONSHIP ( 'NONE' , 'NONE' ,  #14632, #13479 ) ;
#7808 = CARTESIAN_POINT ( 'NONE',  ( 43.01140435219951996, 10.71049967264875491, 29.21067981925357060 ) ) ;
#7809 = PLANE ( 'NONE',  #17114 ) ;
#7810 = CARTESIAN_POINT ( 'NONE',  ( 38.58424406990784661, 135.5297705074273154, 35.64915139335016647 ) ) ;
#7811 = CARTESIAN_POINT ( 'NONE',  ( 15.82680954991375621, 98.96776360684994245, 0.3584833779906905771 ) ) ;
#7812 = CARTESIAN_POINT ( 'NONE',  ( 38.58424406990786082, 123.1151871740940038, 34.21067981925357060 ) ) ;
#7813 = EDGE_CURVE ( 'NONE', #15014, #16099, #11649, .T. ) ;
#7814 = PLANE ( 'NONE',  #19777 ) ;
#7816 = PLANE ( 'NONE',  #10148 ) ;
#7815 = AXIS2_PLACEMENT_3D ( 'NONE', #8746, #12036, #20319 ) ;
#7817 = CARTESIAN_POINT ( 'NONE',  ( 43.01140435219951996, 148.4604996726487798, 39.21067981925356349 ) ) ;
#7818 = CARTESIAN_POINT ( 'NONE',  ( 59.59119729515064279, 96.99641097138604096, 19.72329267725583080 ) ) ;
#7819 = CARTESIAN_POINT ( 'NONE',  ( -151.4692556286852891, -186.2391397928655010, 39.65701158161630246 ) ) ;
#7820 = VECTOR ( 'NONE', #16161, 1000.000000000000000 ) ;
#7821 = CARTESIAN_POINT ( 'NONE',  ( 43.01140435219951286, 107.3651871740940038, 29.55568802177586463 ) ) ;
#7822 = ORIENTED_EDGE ( 'NONE', *, *, #5675, .F. ) ;
#7823 = DIRECTION ( 'NONE',  ( 0.000000000000000000, 1.000000000000000000, 0.000000000000000000 ) ) ;
#7824 = ORIENTED_EDGE ( 'NONE', *, *, #10237, .F. ) ;
#7825 = CARTESIAN_POINT ( 'NONE',  ( 38.96631938032478359, 83.48445800887257917, 31.27175355779120025 ) ) ;
#7826 = LINE ( 'NONE', #16396, #3496 ) ;
#7827 = AXIS2_PLACEMENT_3D ( 'NONE', #122, #16647, #1557 ) ;
#7828 = VECTOR ( 'NONE', #5394, 1000.000000000000000 ) ;
#7829 = CARTESIAN_POINT ( 'NONE',  ( 39.92123440845004723, 148.1604996726487400, 38.46393386101376421 ) ) ;
#7831 = CARTESIAN_POINT ( 'NONE',  ( 70.81223827124823345, 124.1306694702586100, -7.505929917039384058 ) ) ;
#7830 = CARTESIAN_POINT ( 'NONE',  ( 43.01140435219951286, 110.3651871740939754, 29.55568802177586463 ) ) ;
#7832 = CARTESIAN_POINT ( 'NONE',  ( 38.01140435219952707, 63.71049967264874425, 34.21067981925357060 ) ) ;
#7834 = CARTESIAN_POINT ( 'NONE',  ( -148.3790856849358306, -182.4630981290893033, 40.14644641866477315 ) ) ;
#7833 = CARTESIAN_POINT ( 'NONE',  ( 83.67254549292280785, -61.68114226949890622, 10.00000000000001599 ) ) ;
#7835 = SURFACE_STYLE_USAGE ( .BOTH. , #19293 ) ;
#7836 = FACE_OUTER_BOUND ( 'NONE', #20058, .T. ) ;
#7837 = CARTESIAN_POINT ( 'NONE',  ( -161.4692556286852891, -190.4130981290892919, 52.90620854394536821 ) ) ;
#7838 = CARTESIAN_POINT ( 'NONE',  ( 44.37947211624943833, 158.4797705074273040, 30.00020018409699318 ) ) ;
#7839 = CARTESIAN_POINT ( 'NONE',  ( 8.779377865064803999, 119.6051361893432130, -4.922546661887801100 ) ) ;
#7840 = CARTESIAN_POINT ( 'NONE',  ( 41.64333658814960870, 152.5151871740940237, 30.00020018409699318 ) ) ;
#7841 = CARTESIAN_POINT ( 'NONE',  ( 43.01140435219957681, 94.46049967264876557, 39.21067981925356349 ) ) ;
#7842 = CARTESIAN_POINT ( 'NONE',  ( -145.6429501568359797, -168.8438272943107563, 57.67623309621198047 ) ) ;
#7843 = CARTESIAN_POINT ( 'NONE',  ( -160.8964159109769696, -182.3084106276440650, 46.59394152635518083 ) ) ;
#7844 = ORIENTED_EDGE ( 'NONE', *, *, #10163, .F. ) ;
#7845 = CARTESIAN_POINT ( 'NONE',  ( 38.58424406990785371, 66.26518717409400949, 35.64915139335015937 ) ) ;
#7846 = CARTESIAN_POINT ( 'NONE',  ( -148.5561028927606344, -169.2584106276440536, 58.62277379824867296 ) ) ;
#7847 = CARTESIAN_POINT ( 'NONE',  ( 14.94030450088465400, 100.1727563578744196, 14.40630071170483362 ) ) ;
#7848 = DIRECTION ( 'NONE',  ( -0.8660254037844383745, 0.000000000000000000, 0.5000000000000004441 ) ) ;
#7849 = CARTESIAN_POINT ( 'NONE',  ( 45.74753988029933538, 131.0651871740940067, 30.44471234641811819 ) ) ;
#7850 = EDGE_CURVE ( 'NONE', #19966, #4862, #18268, .T. ) ;
#7851 = ORIENTED_EDGE ( 'NONE', *, *, #15967, .T. ) ;
#7852 = ORIENTED_EDGE ( 'NONE', *, *, #905, .T. ) ;
#7853 = CARTESIAN_POINT ( 'NONE',  ( 20.72232308940363765, 137.1362251821529696, 16.90007324815861267 ) ) ;
#7854 = ORIENTED_EDGE ( 'NONE', *, *, #12229, .T. ) ;
#7855 = CARTESIAN_POINT ( 'NONE',  ( 44.55648932407425633, 115.8844580088725991, 29.45539723777780239 ) ) ;
#7856 = DIRECTION ( 'NONE',  ( 0.000000000000000000, 0.000000000000000000, 1.000000000000000000 ) ) ;
#7857 = CARTESIAN_POINT ( 'NONE',  ( 38.58424406990784661, 72.22977050742733240, 32.77220824515698183 ) ) ;
#7858 = CARTESIAN_POINT ( 'NONE',  ( 44.37947211624943833, 140.2151871740940123, 30.00020018409699318 ) ) ;
#7859 =( BOUNDED_CURVE ( )  B_SPLINE_CURVE ( 2, ( #3945, #12423, #15517, #420, #7152, #10672, #17375, #13855, #15731, #635, #5477, #7371, #12203 ),
 .UNSPECIFIED., .F., .F. ) 
 B_SPLINE_CURVE_WITH_KNOTS ( ( 3, 2, 2, 2, 2, 2, 3 ),
 ( 0.5535714285714286031, 0.5571428571428571619, 0.5642857142857142794, 0.5714285714285713969, 0.5785714285714286254, 0.5857142857142857428, 0.5892857142857143016 ),
 .UNSPECIFIED. ) 
 CURVE ( )  GEOMETRIC_REPRESENTATION_ITEM ( )  RATIONAL_B_SPLINE_CURVE ( ( 0.9755282581475768211, 0.9755282581475768211, 1.000000000000000000, 0.9510565162951535312, 1.000000000000000000, 0.9510565162951535312, 1.000000000000000000, 0.9510565162951535312, 1.000000000000000000, 0.9510565162951535312, 1.000000000000000000, 0.9755282581475768211, 0.9755282581475768211 ) ) 
 REPRESENTATION_ITEM ( '' )  );
#7860 = CARTESIAN_POINT ( 'NONE',  ( 39.92123440845004723, 91.16049967264872578, 38.46393386101376421 ) ) ;
#7861 = CARTESIAN_POINT ( 'NONE',  ( 66.24914683137549787, 94.76885710642066840, 6.506024766557033878 ) ) ;
#7862 = EDGE_CURVE ( 'NONE', #10374, #19742, #911, .T. ) ;
#7863 = CARTESIAN_POINT ( 'NONE',  ( -134.9004869860375777, 755.4811543468929358, -3.999999999999980904 ) ) ;
#7864 = CARTESIAN_POINT ( 'NONE',  ( -143.3790856849358306, -162.6891397928654897, 43.77915905869157598 ) ) ;
#7865 = CARTESIAN_POINT ( 'NONE',  ( 46.10157429594899270, 150.8344580088725593, 38.46393386101375711 ) ) ;
#7866 = CARTESIAN_POINT ( 'NONE',  ( -161.4692556286853176, -185.4891397928654726, 49.65701158161630957 ) ) ;
#7867 = ORIENTED_EDGE ( 'NONE', *, *, #10504, .T. ) ;
#7868 = CARTESIAN_POINT ( 'NONE',  ( 44.37947211624943833, 73.27977050742731535, 38.42115945441014446 ) ) ;
#7869 = CARTESIAN_POINT ( 'NONE',  ( -154.3824083646099439, -193.5584106276440650, 58.62277379824867296 ) ) ;
#7870 = EDGE_CURVE ( 'NONE', #14442, #14572, #13089, .T. ) ;
#7871 = CARTESIAN_POINT ( 'NONE',  ( 75.80354157443048280, 110.0810758630161672, 5.910575721798123183 ) ) ;
#7872 = CARTESIAN_POINT ( 'NONE',  ( -142.0420953463935803, -186.8084106276440650, 52.72008163687743831 ) ) ;
#7873 = ORIENTED_EDGE ( 'NONE', *, *, #11424, .F. ) ;
#7874 = CARTESIAN_POINT ( 'NONE',  ( -157.6495955161842062, -161.9391397928654897, 41.15050349809589392 ) ) ;
#7875 = LINE ( 'NONE', #19437, #19778 ) ;
#7876 = CARTESIAN_POINT ( 'NONE',  ( 38.58424406990785371, 120.2297705074273182, 32.77220824515697473 ) ) ;
#7877 = EDGE_CURVE ( 'NONE', #20239, #10293, #9724, .T. ) ;
#7878 = ORIENTED_EDGE ( 'NONE', *, *, #16764, .F. ) ;
#7879 = DIRECTION ( 'NONE',  ( 0.000000000000000000, 1.000000000000000000, 0.000000000000000000 ) ) ;
#7880 = ORIENTED_EDGE ( 'NONE', *, *, #11878, .F. ) ;
#7881 = CARTESIAN_POINT ( 'NONE',  ( 39.42975644700377558, 126.6797705074273210, 36.81289934271958941 ) ) ;
#7882 = LINE ( 'NONE', #7775, #5856 ) ;
#7883 = CARTESIAN_POINT ( 'NONE',  ( 44.55648932407425633, 66.68445800887256780, 38.96596240072933170 ) ) ;
#7884 = DIRECTION ( 'NONE',  ( -0.000000000000000000, -0.000000000000000000, -1.000000000000000000 ) ) ;
#7885 = CARTESIAN_POINT ( 'NONE',  ( 39.92123440845005433, 101.3344580088725877, 29.95742577749336988 ) ) ;
#7886 = CARTESIAN_POINT ( 'NONE',  ( -151.4692556286852891, -177.2391397928654442, 39.65701158161629536 ) ) ;
#7887 = CARTESIAN_POINT ( 'NONE',  ( -145.2889157411863721, -193.4391397928654328, 58.16351966513671812 ) ) ;
#7888 = CYLINDRICAL_SURFACE ( 'NONE', #6610, 21.47274291077713571 ) ;
#7889 = CARTESIAN_POINT ( 'NONE',  ( -81.10645082872859746, 10.96617311717548837, 4.000000000000021316 ) ) ;
#7890 = CARTESIAN_POINT ( 'NONE',  ( -154.3824083646099439, -187.2938272943107449, 58.62277379824867296 ) ) ;
#7891 = EDGE_CURVE ( 'NONE', #4603, #10374, #15355, .T. ) ;
#7892 = CARTESIAN_POINT ( 'NONE',  ( 44.55648932407425633, 124.8844580088725706, 29.45539723777780239 ) ) ;
#7893 = CARTESIAN_POINT ( 'NONE',  ( 47.43856463449118621, 100.8797705074273239, 34.21067981925357060 ) ) ;
#7894 = CARTESIAN_POINT ( 'NONE',  ( 24.78883071187807730, 141.3519591882296709, -10.86778418981948846 ) ) ;
#7895 = CARTESIAN_POINT ( 'NONE',  ( -160.8964159109769696, -181.8938272943107108, 49.65701158161630957 ) ) ;
#7896 = CARTESIAN_POINT ( 'NONE',  ( 38.58424406990785371, 99.26518717409398107, 35.64915139335015937 ) ) ;
#7897 = CARTESIAN_POINT ( 'NONE',  ( 41.46631938032478359, 85.31049967264874567, 38.96596240072933170 ) ) ;
#7898 = EDGE_LOOP ( 'NONE', ( #11171, #6643, #15658, #3321 ) ) ;
#7899 = LINE ( 'NONE', #12846, #17502 ) ;
#7900 = CARTESIAN_POINT ( 'NONE',  ( 47.30009524607925897, 85.94413156685014599, 0.1962900075584997628 ) ) ;
#7901 = CARTESIAN_POINT ( 'NONE',  ( 66.22715431465987024, 135.7747266163150073, -15.00590082692269078 ) ) ;
#7902 = CARTESIAN_POINT ( 'NONE',  ( 45.74753988029934249, 65.32977050742731251, 30.44471234641812174 ) ) ;
#7903 = ORIENTED_EDGE ( 'NONE', *, *, #18515, .F. ) ;
#7904 = ORIENTED_EDGE ( 'NONE', *, *, #7751, .F. ) ;
#7905 = CARTESIAN_POINT ( 'NONE',  ( 38.58424406990784661, 156.5297705074272869, 35.64915139335016647 ) ) ;
#7906 = DIRECTION ( 'NONE',  ( 0.9999746145782334450, -0.007125320983191549967, 0.000000000000000000 ) ) ;
#7907 = AXIS2_PLACEMENT_3D ( 'NONE', #12782, #15866, #5946 ) ;
#7908 = EDGE_CURVE ( 'NONE', #16205, #2985, #16528, .T. ) ;
#7909 = EDGE_CURVE ( 'NONE', #13720, #2548, #21474, .T. ) ;
#7910 = CARTESIAN_POINT ( 'NONE',  ( 43.01140435219951286, 110.9604996726487371, 28.95336869806222779 ) ) ;
#7911 = CARTESIAN_POINT ( 'NONE',  ( 38.58424406990784661, 69.26518717409398107, 35.64915139335016647 ) ) ;
#7912 = LINE ( 'NONE', #9786, #7820 ) ;
#7913 = CARTESIAN_POINT ( 'NONE',  ( -148.5561028927606344, -167.7938272943107165, 40.69124936498395328 ) ) ;
#7914 = DIRECTION ( 'NONE',  ( -0.000000000000000000, -0.000000000000000000, 1.000000000000000000 ) ) ;
#7915 = CARTESIAN_POINT ( 'NONE',  ( -143.3790856849358306, -179.7630981290893146, 43.77915905869157598 ) ) ;
#7916 = CARTESIAN_POINT ( 'NONE',  ( -176.9699209214867608, -126.9891397928655010, 67.64809332337415526 ) ) ;
#7917 = CARTESIAN_POINT ( 'NONE',  ( 41.46631938032478359, 155.1844580088725820, 29.45539723777780239 ) ) ;
#7918 = CARTESIAN_POINT ( 'NONE',  ( 45.74753988029933538, 137.3297705074273267, 30.44471234641811819 ) ) ;
#7919 = CARTESIAN_POINT ( 'NONE',  ( 71.22865828484523831, 100.3801644121689094, 12.26314743512348926 ) ) ;
#7920 = CARTESIAN_POINT ( 'NONE',  ( 47.43856463449117911, 130.7651871740939953, 32.77220824515697473 ) ) ;
#7921 = CARTESIAN_POINT ( 'NONE',  ( -160.8964159109769696, -158.3084106276440650, 46.59394152635518083 ) ) ;
#7922 = LINE ( 'NONE', #2838, #6626 ) ;
#7923 = DIRECTION ( 'NONE',  ( -1.000000000000000000, 0.000000000000000000, 0.000000000000000000 ) ) ;
#7924 = CARTESIAN_POINT ( 'NONE',  ( 71.19430100617981338, 118.9508470517051535, -8.295922056425867552 ) ) ;
#7925 = EDGE_CURVE ( 'NONE', #2439, #17969, #18798, .T. ) ;
#7926 = LINE ( 'NONE', #17827, #9342 ) ;
#7927 = ORIENTED_EDGE ( 'NONE', *, *, #12549, .T. ) ;
#7928 = CARTESIAN_POINT ( 'NONE',  ( 43.01140435219951996, 10.71049967264875491, 34.21067981925357060 ) ) ;
#7929 = ORIENTED_EDGE ( 'NONE', *, *, #17003, .F. ) ;
#7930 = CARTESIAN_POINT ( 'NONE',  ( 41.46631938032478359, 84.38445800887258486, 38.96596240072933170 ) ) ;
#7931 = CARTESIAN_POINT ( 'NONE',  ( 43.80332655382220253, 103.9575765865522925, 29.21067981925356705 ) ) ;
#7932 = EDGE_CURVE ( 'NONE', #16648, #6540, #18152, .T. ) ;
#7933 = CARTESIAN_POINT ( 'NONE',  ( 38.01140435219952707, 153.7104996726487514, 34.21067981925357060 ) ) ;
#7935 = CARTESIAN_POINT ( 'NONE',  ( 15.79683473163509966, 126.9851207307152521, 3.446356185820485418 ) ) ;
#7934 = CARTESIAN_POINT ( 'NONE',  ( 47.43856463449117200, 97.46518717409399812, 35.64915139335016647 ) ) ;
#7936 = CARTESIAN_POINT ( 'NONE',  ( -157.2955611005346270, -163.7084106276440139, 57.67623309621198047 ) ) ;
#7937 = CARTESIAN_POINT ( 'NONE',  ( 39.92123440845004723, 61.16049967264873288, 38.46393386101376421 ) ) ;
#7939 = CARTESIAN_POINT ( 'NONE',  ( 46.10157429594899270, 69.83445800887255928, 38.46393386101375711 ) ) ;
#7938 = DIRECTION ( 'NONE',  ( -1.000000000000000000, 0.000000000000000000, 0.000000000000000000 ) ) ;
#7940 = CARTESIAN_POINT ( 'NONE',  ( -154.5594255724347761, -188.1630981290893203, 40.14644641866476604 ) ) ;
#7941 = LINE ( 'NONE', #9600, #10806 ) ;
#7942 = CARTESIAN_POINT ( 'NONE',  ( 47.43856463449117200, 64.76518717409400949, 32.77220824515698183 ) ) ;
#7943 = CARTESIAN_POINT ( 'NONE',  ( 39.42188022582085694, 153.9507182763122159, -10.27990332573616961 ) ) ;
#7944 = EDGE_CURVE ( 'NONE', #497, #16415, #20983, .T. ) ;
#7945 = CARTESIAN_POINT ( 'NONE',  ( 40.27526882409969744, 150.5651871740940067, 37.97664729208901235 ) ) ;
#7946 = FACE_OUTER_BOUND ( 'NONE', #2821, .T. ) ;
#7947 = VECTOR ( 'NONE', #15174, 1000.000000000000341 ) ;
#7948 = CARTESIAN_POINT ( 'NONE',  ( -145.6429501568359797, -171.8438272943107279, 57.67623309621198047 ) ) ;
#7949 = CARTESIAN_POINT ( 'NONE',  ( -157.2955611005345986, -187.7084106276440139, 57.67623309621197336 ) ) ;
#7950 = ORIENTED_EDGE ( 'NONE', *, *, #21656, .T. ) ;
#7951 = CARTESIAN_POINT ( 'NONE',  ( 47.43856463449117911, 64.76518717409400949, 32.77220824515697473 ) ) ;
#7952 = CARTESIAN_POINT ( 'NONE',  ( -143.8425227516148084, -165.3584106276440480, 44.11586579668791330 ) ) ;
#7953 = CARTESIAN_POINT ( 'NONE',  ( 65.15795615308765321, 146.1170287843621054, 17.62046751038700165 ) ) ;
#7954 = DIRECTION ( 'NONE',  ( 0.000000000000000000, 0.000000000000000000, 1.000000000000000000 ) ) ;
#7955 = CARTESIAN_POINT ( 'NONE',  ( 47.43856463449117200, 133.4651871740940123, 35.64915139335016647 ) ) ;
#7956 = CARTESIAN_POINT ( 'NONE',  ( 51.37827275082728562, 86.79484443300951568, -12.94217320967262275 ) ) ;
#7957 = ORIENTED_EDGE ( 'NONE', *, *, #2069, .T. ) ;
#7958 = CARTESIAN_POINT ( 'NONE',  ( 151.4773229304660731, 84.89323405393692212, 4.000000000000021316 ) ) ;
#7959 = ORIENTED_EDGE ( 'NONE', *, *, #11706, .T. ) ;
#7960 = CARTESIAN_POINT ( 'NONE',  ( 43.80332655382220253, 59.88361825032847463, 29.21067981925356705 ) ) ;
#7961 = AXIS2_PLACEMENT_3D ( 'NONE', #5334, #20552, #20229 ) ;
#7962 = CARTESIAN_POINT ( 'NONE',  ( 41.64333658814960870, 77.77977050742731535, 30.00020018409699318 ) ) ;
#7964 = CARTESIAN_POINT ( 'NONE',  ( 37.00104444766353851, 92.35499785847434850, 7.656504971210453370 ) ) ;
#7963 = CARTESIAN_POINT ( 'NONE',  ( 46.59305225739526435, 139.9151871740940010, 31.60846029578754468 ) ) ;
#7965 = CARTESIAN_POINT ( 'NONE',  ( 41.46631938032478359, 88.31049967264874567, 38.96596240072933170 ) ) ;
#7966 = CARTESIAN_POINT ( 'NONE',  ( 75.40436159597490473, 130.9804297329818326, 12.22031048084446248 ) ) ;
#7967 = AXIS2_PLACEMENT_3D ( 'NONE', #8982, #4327, #11052 ) ;
#7968 = DIRECTION ( 'NONE',  ( 0.000000000000000000, 0.000000000000000000, 1.000000000000000000 ) ) ;
#7969 = CARTESIAN_POINT ( 'NONE',  ( -141.4692556286852891, -159.8391397928654385, 46.40781461928724383 ) ) ;
#7970 = CARTESIAN_POINT ( 'NONE',  ( 45.74753988029933538, 92.06518717409399244, 30.44471234641811819 ) ) ;
#7971 = CARTESIAN_POINT ( 'NONE',  ( 42.35458290462738518, 144.9005011087681396, 39.17808643222355869 ) ) ;
#7972 = CARTESIAN_POINT ( 'NONE',  ( 44.55648932407425633, 108.6844580088725820, 38.96596240072933170 ) ) ;
#7973 = CARTESIAN_POINT ( 'NONE',  ( 46.10157429594899270, 141.8344580088725593, 38.46393386101375711 ) ) ;
#7974 = ORIENTED_EDGE ( 'NONE', *, *, #17933, .T. ) ;
#7975 = CARTESIAN_POINT ( 'NONE',  ( 40.27526882409969033, 77.92977050742732104, 30.44471234641811819 ) ) ;
#7976 = CARTESIAN_POINT ( 'NONE',  ( -145.6429501568359797, -192.2084106276440139, 41.63779006702063867 ) ) ;
#7977 = CARTESIAN_POINT ( 'NONE',  ( 76.92284642892752800, 124.5854180935290714, 5.434424407683230207 ) ) ;
#7978 = CARTESIAN_POINT ( 'NONE',  ( -148.5561028927606344, -184.2584106276440536, 58.62277379824867296 ) ) ;
#7979 = ORIENTED_EDGE ( 'NONE', *, *, #1718, .F. ) ;
#7980 = CARTESIAN_POINT ( 'NONE',  ( 39.42975644700377558, 158.8151871740940067, 31.60846029578754468 ) ) ;
#7981 = AXIS2_PLACEMENT_3D ( 'NONE', #15026, #151, #10193 ) ;
#7982 = EDGE_CURVE ( 'NONE', #10538, #20193, #18381, .T. ) ;
#7983 = LINE ( 'NONE', #10072, #12722 ) ;
#7984 = CARTESIAN_POINT ( 'NONE',  ( 47.43856463449117911, 128.0297705074273154, 32.77220824515697473 ) ) ;
#7985 = ORIENTED_EDGE ( 'NONE', *, *, #12830, .T. ) ;
#7986 = CARTESIAN_POINT ( 'NONE',  ( 46.10157429594899270, 87.83445800887255928, 38.46393386101375711 ) ) ;
#7987 =( BOUNDED_CURVE ( )  B_SPLINE_CURVE ( 2, ( #21214, #16342, #8206, #1474, #14907, #4438, #8093, #16449, #14800, #1362, #12717, #1037, #21541 ),
 .UNSPECIFIED., .F., .F. ) 
 B_SPLINE_CURVE_WITH_KNOTS ( ( 3, 2, 2, 2, 2, 2, 3 ),
 ( 0.2720588235294117974, 0.2735294117647059098, 0.2764705882352941346, 0.2794117647058823595, 0.2823529411764705843, 0.2852941176470588092, 0.2867647058823529216 ),
 .UNSPECIFIED. ) 
 CURVE ( )  GEOMETRIC_REPRESENTATION_ITEM ( )  RATIONAL_B_SPLINE_CURVE ( ( 0.9755282581475768211, 0.9755282581475772652, 1.000000000000000000, 0.9510565162951535312, 1.000000000000000000, 0.9510565162951535312, 1.000000000000000000, 0.9510565162951535312, 1.000000000000000000, 0.9510565162951535312, 1.000000000000000000, 0.9755282581475768211, 0.9755282581475768211 ) ) 
 REPRESENTATION_ITEM ( '' )  );
#7988 = ORIENTED_EDGE ( 'NONE', *, *, #14486, .T. ) ;
#7989 = CARTESIAN_POINT ( 'NONE',  ( 43.01140435219951286, 115.1297705074272955, 38.86567161673127657 ) ) ;
#7990 = CARTESIAN_POINT ( 'NONE',  ( 43.01140435219951286, 99.53445800887257633, 39.21067981925356349 ) ) ;
#7991 = CARTESIAN_POINT ( 'NONE',  ( 47.43856463449117200, 88.72977050742730398, 35.64915139335016647 ) ) ;
#7992 = CARTESIAN_POINT ( 'NONE',  ( 41.46631938032478359, 65.18445800887258201, 29.45539723777780239 ) ) ;
#7993 = VECTOR ( 'NONE', #5993, 1000.000000000000000 ) ;
#7994 = DIRECTION ( 'NONE',  ( 0.9385982292947087080, 0.3450121214752278620, -2.040824802394967678E-16 ) ) ;
#7995 = CARTESIAN_POINT ( 'NONE',  ( 38.96631938032478359, 83.48445800887257917, 31.27175355779120025 ) ) ;
#7996 = CARTESIAN_POINT ( 'NONE',  ( 41.46631938032478359, 96.11049967264874283, 29.45539723777780239 ) ) ;
#7997 = CARTESIAN_POINT ( 'NONE',  ( -143.3790856849358306, -189.6891397928654612, 43.77915905869157598 ) ) ;
#7998 = DIRECTION ( 'NONE',  ( -1.140132994654635861E-16, -0.000000000000000000, -1.000000000000000000 ) ) ;
#7999 = CARTESIAN_POINT ( 'NONE',  ( 41.46631938032478359, 103.3104996726487457, 38.96596240072933170 ) ) ;
#8000 = CARTESIAN_POINT ( 'NONE',  ( -159.0959885057557983, -187.5938272943107279, 55.19815736654470584 ) ) ;
#8001 = CONTEXT_DEPENDENT_SHAPE_REPRESENTATION ( #17294, #10981 ) ;
#8002 = CARTESIAN_POINT ( 'NONE',  ( 38.01140435219951996, 119.6344580088725706, 32.58608133808903773 ) ) ;
#8003 = CARTESIAN_POINT ( 'NONE',  ( 38.58424406990786082, 99.37977050742732388, 34.21067981925357060 ) ) ;
#8004 = CARTESIAN_POINT ( 'NONE',  ( 30.88693878601983300, 94.35661743609990992, 20.91413290821214588 ) ) ;
#8005 = CARTESIAN_POINT ( 'NONE',  ( -143.8425227516148084, -183.0938272943107279, 44.11586579668791330 ) ) ;
#8006 = CARTESIAN_POINT ( 'NONE',  ( 47.43856463449117911, 85.46518717409399812, 35.64915139335015937 ) ) ;
#8007 = CARTESIAN_POINT ( 'NONE',  ( 33.01140435219951286, 119.9070776186055838, -35.00000000000000000 ) ) ;
#8008 = ORIENTED_EDGE ( 'NONE', *, *, #3229, .F. ) ;
#8009 = DIRECTION ( 'NONE',  ( 0.000000000000000000, 1.000000000000000000, 0.000000000000000000 ) ) ;
#8010 = CARTESIAN_POINT ( 'NONE',  ( 30.24639091383375700, 151.6717570033048048, 3.410403464249057492 ) ) ;
#8011 = CARTESIAN_POINT ( 'NONE',  ( 38.58424406990786082, 144.3797705074273097, 34.21067981925357060 ) ) ;
#8012 = CARTESIAN_POINT ( 'NONE',  ( 14.85320491933239317, 121.4429315054255909, 16.22795414098078126 ) ) ;
#8013 = PRODUCT ( 'Lower Fixed Base Shear Blade', 'Lower Fixed Base Shear Blade', '', ( #5784 ) ) ;
#8014 = CARTESIAN_POINT ( 'NONE',  ( 38.58424406990785371, 66.52977050742731535, 35.64915139335015937 ) ) ;
#8015 = VERTEX_POINT ( 'NONE', #12411 ) ;
#8016 = ORIENTED_EDGE ( 'NONE', *, *, #17394, .T. ) ;
#8017 = CARTESIAN_POINT ( 'NONE',  ( 43.01140435219951286, 157.1297705074272812, 38.86567161673127657 ) ) ;
#8019 = ADVANCED_FACE ( 'NONE', ( #5688 ), #943, .F. ) ;
#8018 = CARTESIAN_POINT ( 'NONE',  ( -94.10404323627655288, -13.18023274290474767, 4.000000000000021316 ) ) ;
#8020 = AXIS2_PLACEMENT_3D ( 'NONE', #49, #17011, #11727 ) ;
#8021 = CARTESIAN_POINT ( 'NONE',  ( 38.96631938032478359, 112.0104996726487485, 37.14960608071593384 ) ) ;
#8022 = CARTESIAN_POINT ( 'NONE',  ( 38.58424406990786082, 66.11518717409398960, 34.21067981925357060 ) ) ;
#8023 = CARTESIAN_POINT ( 'NONE',  ( -160.8964159109769696, -160.7438272943107336, 52.72008163687743121 ) ) ;
#8024 = VECTOR ( 'NONE', #18677, 1000.000000000000114 ) ;
#8025 = CARTESIAN_POINT ( 'NONE',  ( 111.4021762516569964, 137.5714195593754710, -35.00000000000000000 ) ) ;
#8026 = CARTESIAN_POINT ( 'NONE',  ( -151.4692556286852891, -174.8130981290892976, 60.17163382399899518 ) ) ;
#8027 = CARTESIAN_POINT ( 'NONE',  ( 43.01140435219951286, 149.0344580088725763, 28.95336869806222779 ) ) ;
#8028 = CARTESIAN_POINT ( 'NONE',  ( 44.37947211624943833, 136.2797705074273154, 38.42115945441014446 ) ) ;
#8029 = CARTESIAN_POINT ( 'NONE',  ( 11.40453246296876877, 106.5480838228176452, 14.64419766361223552 ) ) ;
#8030 = CARTESIAN_POINT ( 'NONE',  ( 45.74753988029934249, 125.0651871740939924, 30.44471234641812174 ) ) ;
#8031 = CARTESIAN_POINT ( 'NONE',  ( -154.5594255724347761, -168.0891397928654669, 40.14644641866476604 ) ) ;
#8032 = CARTESIAN_POINT ( 'NONE',  ( -154.3824083646099439, -160.5584106276440366, 58.62277379824867296 ) ) ;
#8033 = DIRECTION ( 'NONE',  ( 0.000000000000000000, 1.000000000000000000, 0.000000000000000000 ) ) ;
#8034 = CARTESIAN_POINT ( 'NONE',  ( 43.01140435219951996, 149.9604996726487798, 29.21067981925357060 ) ) ;
#8035 = CARTESIAN_POINT ( 'NONE',  ( 50.58784882905466418, 147.1537178454131549, 17.22345644918840790 ) ) ;
#8036 = CARTESIAN_POINT ( 'NONE',  ( 48.01140435219951996, 83.06049967264873146, 35.83527830041809636 ) ) ;
#8037 = EDGE_CURVE ( 'NONE', #8122, #21618, #11078, .T. ) ;
#8038 = EDGE_CURVE ( 'NONE', #7658, #19406, #6477, .T. ) ;
#8039 = ORIENTED_EDGE ( 'NONE', *, *, #11781, .F. ) ;
#8040 = CIRCLE ( 'NONE', #6650, 10.00000000000000888 ) ;
#8041 = EDGE_LOOP ( 'NONE', ( #4541, #4091, #16197, #8955, #21027, #16222, #15590, #21733, #20879, #1225, #8451, #2175, #17182, #20537, #15801, #16723, #12711, #20352 ) ) ;
#8042 = CARTESIAN_POINT ( 'NONE',  ( 43.01140435219951286, 78.53445800887259054, 39.46799094044489209 ) ) ;
#8043 = CARTESIAN_POINT ( 'NONE',  ( 44.55648932407425633, 103.8844580088725849, 29.45539723777780239 ) ) ;
#8044 = CARTESIAN_POINT ( 'NONE',  ( 48.01140435219951996, 140.0604996726487457, 35.83527830041810347 ) ) ;
#8046 = CARTESIAN_POINT ( 'NONE',  ( 53.81137604271221164, 145.8702381773545653, 5.351212940250758443 ) ) ;
#8045 = CARTESIAN_POINT ( 'NONE',  ( 46.59305225739526435, 100.3151871740940067, 36.81289934271958941 ) ) ;
#8047 = DIRECTION ( 'NONE',  ( 1.000000000000000000, 0.000000000000000000, 0.000000000000000000 ) ) ;
#8048 = CARTESIAN_POINT ( 'NONE',  ( -157.2955611005346270, -167.6084106276440480, 41.63779006702063867 ) ) ;
#8049 = CARTESIAN_POINT ( 'NONE',  ( -145.6429501568359797, -194.9438272943107222, 41.63779006702063867 ) ) ;
#8051 = DIRECTION ( 'NONE',  ( -0.9385982292947088190, -0.3450121214752275289, 0.000000000000000000 ) ) ;
#8050 = CARTESIAN_POINT ( 'NONE',  ( -151.4692556286852891, -177.8130981290892976, 59.65701158161631668 ) ) ;
#8052 = CARTESIAN_POINT ( 'NONE',  ( -141.4692556286852891, -176.9130981290892635, 46.40781461928724383 ) ) ;
#8053 = CARTESIAN_POINT ( 'NONE',  ( 43.01140435219951286, 158.6297705074273381, 29.55568802177586463 ) ) ;
#8054 = CARTESIAN_POINT ( 'NONE',  ( -151.4692556286852607, -159.8130981290892692, 59.65701158161632378 ) ) ;
#8055 = CARTESIAN_POINT ( 'NONE',  ( 8.927628897234525240, 116.7075971571176751, 1.981832035706394546 ) ) ;
#8056 = CARTESIAN_POINT ( 'NONE',  ( -142.0420953463935803, -162.2438272943107336, 46.59394152635518793 ) ) ;
#8057 = CARTESIAN_POINT ( 'NONE',  ( -145.6429501568359797, -189.2084106276440423, 41.63779006702063867 ) ) ;
#8058 = ORIENTED_EDGE ( 'NONE', *, *, #11482, .F. ) ;
#8059 = CARTESIAN_POINT ( 'NONE',  ( 44.37947211624943833, 74.21518717409399812, 30.00020018409699318 ) ) ;
#8060 = CARTESIAN_POINT ( 'NONE',  ( -159.0959885057557983, -170.4584106276440423, 44.11586579668791330 ) ) ;
#8061 = CARTESIAN_POINT ( 'NONE',  ( 32.32016755483360271, 87.30015788337030358, 13.69171886368053492 ) ) ;
#8062 = ADVANCED_FACE ( 'NONE', ( #4041 ), #2487, .F. ) ;
#8063 = PLANE ( 'NONE',  #20780 ) ;
#8064 = CARTESIAN_POINT ( 'NONE',  ( 39.42975644700377558, 132.4151871740940010, 36.81289934271958941 ) ) ;
#8065 = EDGE_CURVE ( 'NONE', #13715, #460, #9299, .T. ) ;
#8066 = CARTESIAN_POINT ( 'NONE',  ( 66.55041322599720388, 95.16028120083096553, -6.513516925475251185 ) ) ;
#8067 = ORIENTED_EDGE ( 'NONE', *, *, #9771, .F. ) ;
#8068 = ORIENTED_EDGE ( 'NONE', *, *, #6789, .F. ) ;
#8069 = CARTESIAN_POINT ( 'NONE',  ( 30.72731853479779929, 94.52359049060457608, 14.91853181686295038 ) ) ;
#8070 = ORIENTED_EDGE ( 'NONE', *, *, #21778, .F. ) ;
#8071 = CARTESIAN_POINT ( 'NONE',  ( 43.01140435219951286, 66.53445800887257633, 39.21067981925356349 ) ) ;
#8072 = AXIS2_PLACEMENT_3D ( 'NONE', #5800, #10565, #2280 ) ;
#8073 = CARTESIAN_POINT ( 'NONE',  ( 38.58424406990786082, 66.37977050742730967, 34.21067981925357060 ) ) ;
#8075 = CARTESIAN_POINT ( 'NONE',  ( 47.24326884731692644, 147.7868190896643341, 4.084992211255583427 ) ) ;
#8074 = CARTESIAN_POINT ( 'NONE',  ( 43.01140435219951286, 122.3651871740939754, 29.55568802177586463 ) ) ;
#8076 = CARTESIAN_POINT ( 'NONE',  ( 41.46631938032478359, 91.31049967264874567, 38.96596240072933170 ) ) ;
#8077 = DIRECTION ( 'NONE',  ( -0.000000000000000000, -0.000000000000000000, 1.000000000000000000 ) ) ;
#8078 = DIRECTION ( 'NONE',  ( -0.000000000000000000, -0.000000000000000000, -1.000000000000000000 ) ) ;
#8079 = DIRECTION ( 'NONE',  ( 1.000000000000000000, 0.000000000000000000, 0.000000000000000000 ) ) ;
#8080 = CARTESIAN_POINT ( 'NONE',  ( 40.27526882409969033, 89.66518717409400097, 30.44471234641811819 ) ) ;
#8081 = CARTESIAN_POINT ( 'NONE',  ( 47.05648932407426344, 150.9844580088725934, 37.14960608071593384 ) ) ;
#8082 = DIRECTION ( 'NONE',  ( -0.000000000000000000, 1.000000000000000000, -0.000000000000000000 ) ) ;
#8083 = VERTEX_POINT ( 'NONE', #16030 ) ;
#8084 = CARTESIAN_POINT ( 'NONE',  ( 43.01140435219951286, 77.62977050742729546, 29.55568802177586463 ) ) ;
#8085 = CARTESIAN_POINT ( 'NONE',  ( -159.0959885057557983, -194.4584106276440423, 44.11586579668791330 ) ) ;
#8086 = CARTESIAN_POINT ( 'NONE',  ( 24.41145734808947054, 148.6458414325078081, 10.19629000755267434 ) ) ;
#8087 = CARTESIAN_POINT ( 'NONE',  ( -148.5561028927606344, -181.2584106276440536, 58.62277379824867296 ) ) ;
#8088 = ORIENTED_EDGE ( 'NONE', *, *, #2476, .F. ) ;
#8089 = DIRECTION ( 'NONE',  ( -1.000000000000000000, 0.000000000000000000, 0.000000000000000000 ) ) ;
#8090 = CARTESIAN_POINT ( 'NONE',  ( 43.01140435219951996, 10.71049967264875491, 29.21067981925357060 ) ) ;
#8091 = CARTESIAN_POINT ( 'NONE',  ( 41.64333658814960870, 119.7797705074273296, 30.00020018409699318 ) ) ;
#8092 = VERTEX_POINT ( 'NONE', #9229 ) ;
#8093 = CARTESIAN_POINT ( 'NONE',  ( 48.01140435219951996, 130.2844580088725763, 34.21067981925357060 ) ) ;
#8094 = ORIENTED_EDGE ( 'NONE', *, *, #7191, .T. ) ;
#8095 = CARTESIAN_POINT ( 'NONE',  ( 44.37947211624943833, 119.4797705074273182, 30.00020018409699318 ) ) ;
#8096 = CARTESIAN_POINT ( 'NONE',  ( -151.4692556286852607, -155.3130981290892976, 39.65701158161629536 ) ) ;
#8097 = CARTESIAN_POINT ( 'NONE',  ( 47.43856463449117200, 151.7651871740939669, 32.77220824515698183 ) ) ;
#8098 =( GEOMETRIC_REPRESENTATION_CONTEXT ( 3 ) GLOBAL_UNCERTAINTY_ASSIGNED_CONTEXT ( ( #7758 ) ) GLOBAL_UNIT_ASSIGNED_CONTEXT ( ( #10548, #14265, #17895 ) ) REPRESENTATION_CONTEXT ( 'NONE', 'WORKASPACE' ) );
#8099 = DIRECTION ( 'NONE',  ( 0.8302490056034133037, 0.5573926701119628069, -0.000000000000000000 ) ) ;
#8100 = CARTESIAN_POINT ( 'NONE',  ( 39.92123440845005433, 83.33445800887257349, 29.95742577749336988 ) ) ;
#8101 = CARTESIAN_POINT ( 'NONE',  ( 38.96631938032478359, 96.41049967264873999, 31.27175355779120025 ) ) ;
#8102 = CARTESIAN_POINT ( 'NONE',  ( -161.4692556286853176, -182.4891397928654726, 49.65701158161630957 ) ) ;
#8103 = CARTESIAN_POINT ( 'NONE',  ( 43.01140435219951996, 10.71049967264875491, 29.21067981925357060 ) ) ;
#8104 = CARTESIAN_POINT ( 'NONE',  ( -151.4692556286852607, -172.7391397928654726, 59.65701158161632378 ) ) ;
#8105 = CARTESIAN_POINT ( 'NONE',  ( -157.2955611005346270, -190.4438272943107506, 57.67623309621198047 ) ) ;
#8106 = CARTESIAN_POINT ( 'NONE',  ( 48.01140435219951996, 127.1344580088725706, 35.83527830041810347 ) ) ;
#8107 = CARTESIAN_POINT ( 'NONE',  ( 41.64333658814960870, 101.7797705074273154, 30.00020018409699318 ) ) ;
#8108 = CARTESIAN_POINT ( 'NONE',  ( 64.05606230151549596, 101.0139342820504993, 19.48556066606253978 ) ) ;
#8109 = CARTESIAN_POINT ( 'NONE',  ( -159.0959885057557983, -179.1938272943107506, 44.11586579668791330 ) ) ;
#8110 = CARTESIAN_POINT ( 'NONE',  ( 43.01140435219951286, 84.86518717409400381, 38.86567161673127657 ) ) ;
#8111 = CARTESIAN_POINT ( 'NONE',  ( 43.01140435219951996, 10.71049967264875491, 34.21067981925357060 ) ) ;
#8112 = ORIENTED_EDGE ( 'NONE', *, *, #11528, .F. ) ;
#8113 = CARTESIAN_POINT ( 'NONE',  ( 43.01140435219951996, 10.71049967264875491, 34.21067981925357060 ) ) ;
#8114 = CARTESIAN_POINT ( 'NONE',  ( 23.42018083028975184, 147.9700754799198705, 17.16443675223517573 ) ) ;
#8115 =( BOUNDED_CURVE ( )  B_SPLINE_CURVE ( 2, ( #11893, #3527, #10252, #208, #6946, #20386, #5283, #20498, #11997, #18730, #17061, #1973, #10470 ),
 .UNSPECIFIED., .F., .T. ) 
 B_SPLINE_CURVE_WITH_KNOTS ( ( 3, 2, 2, 2, 2, 2, 3 ),
 ( 0.5178571428571429047, 0.5214285714285714635, 0.5285714285714285809, 0.5357142857142856984, 0.5428571428571428159, 0.5500000000000000444, 0.5535714285714286031 ),
 .UNSPECIFIED. ) 
 CURVE ( )  GEOMETRIC_REPRESENTATION_ITEM ( )  RATIONAL_B_SPLINE_CURVE ( ( 0.9755282581475768211, 0.9755282581475771542, 1.000000000000000000, 0.9510565162951535312, 1.000000000000000000, 0.9510565162951535312, 1.000000000000000000, 0.9510565162951535312, 1.000000000000000000, 0.9510565162951535312, 1.000000000000000000, 0.9755282581475768211, 0.9755282581475768211 ) ) 
 REPRESENTATION_ITEM ( '' )  );
#8116 = CARTESIAN_POINT ( 'NONE',  ( 44.37947211624943833, 145.2797705074273154, 38.42115945441014446 ) ) ;
#8117 = CARTESIAN_POINT ( 'NONE',  ( 64.45983652262509622, 101.7220219035630748, -6.553643814208265361 ) ) ;
#8118 = PRESENTATION_LAYER_ASSIGNMENT (  '', '', ( #15142 ) ) ;
#8119 = EDGE_CURVE ( 'NONE', #15219, #2955, #10768, .T. ) ;
#8120 = CARTESIAN_POINT ( 'NONE',  ( 47.43856463449118621, 67.87977050742730967, 34.21067981925357060 ) ) ;
#8121 = EDGE_LOOP ( 'NONE', ( #10128, #20673, #1578, #1879 ) ) ;
#8122 = VERTEX_POINT ( 'NONE', #19460 ) ;
#8123 = CARTESIAN_POINT ( 'NONE',  ( 47.43856463449117200, 148.7297705074273324, 35.64915139335016647 ) ) ;
#8124 = CARTESIAN_POINT ( 'NONE',  ( 43.01140435219951996, 10.71049967264875491, 39.21067981925356349 ) ) ;
#8125 = CARTESIAN_POINT ( 'NONE',  ( 47.05648932407426344, 112.9104996726487400, 37.14960608071593384 ) ) ;
#8126 = CARTESIAN_POINT ( 'NONE',  ( 44.37947211624943833, 68.21518717409399812, 30.00020018409699318 ) ) ;
#8127 = CARTESIAN_POINT ( 'NONE',  ( -148.5561028927606344, -156.0584106276440650, 40.69124936498395328 ) ) ;
#8128 = CARTESIAN_POINT ( 'NONE',  ( -151.4692556286852891, -158.6438272943107108, 39.74470866294723947 ) ) ;
#8129 = CARTESIAN_POINT ( 'NONE',  ( -154.5594255724347761, -182.1630981290893203, 40.14644641866476604 ) ) ;
#8130 = AXIS2_PLACEMENT_3D ( 'NONE', #16964, #17071, #16751 ) ;
#8131 = EDGE_CURVE ( 'NONE', #16393, #20969, #19854, .T. ) ;
#8132 = CARTESIAN_POINT ( 'NONE',  ( 44.55648932407425633, 150.6844580088725820, 38.96596240072933170 ) ) ;
#8133 = CARTESIAN_POINT ( 'NONE',  ( 44.37947211624943833, 134.4797705074273324, 30.00020018409699318 ) ) ;
#8134 = CARTESIAN_POINT ( 'NONE',  ( 65.15795615308765321, 146.1170287843621054, 17.62046751038700165 ) ) ;
#8135 = CARTESIAN_POINT ( 'NONE',  ( 43.01140435219951286, 120.8651871740940180, 38.86567161673127657 ) ) ;
#8136 = CARTESIAN_POINT ( 'NONE',  ( -157.6495955161842062, -182.0391397928654840, 58.16351966513671812 ) ) ;
#8137 = CARTESIAN_POINT ( 'NONE',  ( 43.01140435219951996, 10.71049967264875491, 9.210679819253577705 ) ) ;
#8138 = CARTESIAN_POINT ( 'NONE',  ( 45.51144763592289877, 59.40255829349017347, 29.88057779030456373 ) ) ;
#8139 = CARTESIAN_POINT ( 'NONE',  ( 31.13415902118537559, 151.9291573665896635, 4.438733124005141306 ) ) ;
#8140 = EDGE_CURVE ( 'NONE', #18529, #5215, #2814, .T. ) ;
#8141 = CARTESIAN_POINT ( 'NONE',  ( 32.78705717043479240, 146.2756902729748560, 16.50925200294354056 ) ) ;
#8142 = CARTESIAN_POINT ( 'NONE',  ( -148.3790856849358306, -187.5891397928654953, 59.16757674456786020 ) ) ;
#8143 = CARTESIAN_POINT ( 'NONE',  ( 38.58424406990785371, 99.52977050742730114, 35.64915139335015937 ) ) ;
#8144 = ORIENTED_EDGE ( 'NONE', *, *, #5733, .F. ) ;
#8145 = EDGE_CURVE ( 'NONE', #18280, #12353, #5974, .T. ) ;
#8146 = CARTESIAN_POINT ( 'NONE',  ( 141.1725454929228079, -61.68114226949890622, -16.21320343559643717 ) ) ;
#8147 = EDGE_LOOP ( 'NONE', ( #17763, #14172, #16091, #14849 ) ) ;
#8148 = CARTESIAN_POINT ( 'NONE',  ( 46.10157429594899270, 85.73445800887256496, 29.95742577749337343 ) ) ;
#8149 = CARTESIAN_POINT ( 'NONE',  ( 2.004595370269653287, 635.3380690778678854, -0.8325491102011938205 ) ) ;
#8150 = CARTESIAN_POINT ( 'NONE',  ( 38.01140435219951996, 135.5604996726487457, 32.58608133808903773 ) ) ;
#8152 = CARTESIAN_POINT ( 'NONE',  ( 25.52315018325464635, 97.88680518890443238, 9.160641959101482712 ) ) ;
#8151 = CARTESIAN_POINT ( 'NONE',  ( 44.37947211624943833, 101.2151871740939981, 30.00020018409699318 ) ) ;
#8153 = CARTESIAN_POINT ( 'NONE',  ( -157.2955611005346270, -172.7084106276440423, 57.67623309621198047 ) ) ;
#8154 = CARTESIAN_POINT ( 'NONE',  ( -160.8964159109769696, -188.0438272943107449, 46.59394152635518083 ) ) ;
#8156 = DIRECTION ( 'NONE',  ( -0.000000000000000000, -0.000000000000000000, -1.000000000000000000 ) ) ;
#8155 = CARTESIAN_POINT ( 'NONE',  ( -157.6495955161842062, -166.1130981290892805, 58.16351966513671812 ) ) ;
#8157 = CARTESIAN_POINT ( 'NONE',  ( 42.21948215057684450, 105.0373810949690210, 29.21067981925356705 ) ) ;
#8158 = AXIS2_PLACEMENT_3D ( 'NONE', #11518, #12276, #3806 ) ;
#8159 = CARTESIAN_POINT ( 'NONE',  ( -151.4692556286852891, -177.8130981290892976, 59.65701158161631668 ) ) ;
#8160 = CARTESIAN_POINT ( 'NONE',  ( 144.5586921005913439, -37.13255853780189852, -19.99999999999999645 ) ) ;
#8161 = CARTESIAN_POINT ( 'NONE',  ( 43.01140435219951286, 157.1297705074272812, 38.86567161673127657 ) ) ;
#8162 = CARTESIAN_POINT ( 'NONE',  ( -157.6495955161842062, -184.1130981290892521, 58.16351966513671812 ) ) ;
#8163 = CARTESIAN_POINT ( 'NONE',  ( 40.90832812944997698, 154.0758954209757121, 3.767805038447253452 ) ) ;
#8164 = CARTESIAN_POINT ( 'NONE',  ( 40.27526882409969744, 147.5651871740939782, 37.97664729208901235 ) ) ;
#8165 = CARTESIAN_POINT ( 'NONE',  ( -160.8964159109769696, -157.7438272943107336, 52.72008163687743121 ) ) ;
#8166 = CARTESIAN_POINT ( 'NONE',  ( -159.0959885057557983, -184.8584106276440480, 55.19815736654470584 ) ) ;
#8167 = EDGE_CURVE ( 'NONE', #2361, #5629, #17793, .T. ) ;
#8168 = EDGE_LOOP ( 'NONE', ( #7878, #3342, #6283, #7123 ) ) ;
#8169 = CARTESIAN_POINT ( 'NONE',  ( 41.64333658814960870, 71.51518717409399528, 30.00020018409699318 ) ) ;
#8170 = CARTESIAN_POINT ( 'NONE',  ( -148.5561028927606344, -174.0584106276440366, 40.69124936498395328 ) ) ;
#8171 = CARTESIAN_POINT ( 'NONE',  ( 34.18339000214019308, 153.0669919960894845, 16.54886172077450368 ) ) ;
#8172 = CARTESIAN_POINT ( 'NONE',  ( 43.01140435219951996, 10.71049967264875491, 29.21067981925357060 ) ) ;
#8173 = CARTESIAN_POINT ( 'NONE',  ( 38.58424406990786082, 120.1151871740940038, 34.21067981925357060 ) ) ;
#8174 = CARTESIAN_POINT ( 'NONE',  ( 23.40005864183818218, 147.8691531402271835, -9.846981161663094895 ) ) ;
#8175 = EDGE_LOOP ( 'NONE', ( #14150, #17505 ) ) ;
#8176 = VERTEX_POINT ( 'NONE', #14171 ) ;
#8177 = AXIS2_PLACEMENT_3D ( 'NONE', #2454, #2666, #14354 ) ;
#8178 =( REPRESENTATION_RELATIONSHIP ('NONE','NONE', #6933, #6206 ) REPRESENTATION_RELATIONSHIP_WITH_TRANSFORMATION ( #20126 )SHAPE_REPRESENTATION_RELATIONSHIP( ) );
#8179 = CARTESIAN_POINT ( 'NONE',  ( 38.01140435219952707, 113.9344580088725820, 35.83527830041809636 ) ) ;
#8180 = EDGE_LOOP ( 'NONE', ( #3569, #6981, #14017, #16784, #14990, #8511, #17439, #14801 ) ) ;
#8181 = EDGE_CURVE ( 'NONE', #17373, #5984, #4180, .T. ) ;
#8182 = CARTESIAN_POINT ( 'NONE',  ( 38.96631938032478359, 110.4844580088725792, 31.27175355779120025 ) ) ;
#8183 = CARTESIAN_POINT ( 'NONE',  ( 43.01140435219951996, 70.71049967264875136, 29.21067981925357060 ) ) ;
#8184 = CIRCLE ( 'NONE', #8539, 10.00000000000000888 ) ;
#8185 = CARTESIAN_POINT ( 'NONE',  ( 45.74753988029933538, 64.42977050742732104, 37.97664729208901946 ) ) ;
#8187 = CARTESIAN_POINT ( 'NONE',  ( 69.49396330798431620, 129.5978393632817927, 5.275421687385184910 ) ) ;
#8186 = CARTESIAN_POINT ( 'NONE',  ( 44.37947211624943833, 125.2151871740939981, 30.00020018409699318 ) ) ;
#8188 = CARTESIAN_POINT ( 'NONE',  ( 48.01140435219951996, 83.21049967264873715, 34.21067981925357060 ) ) ;
#8189 = DIRECTION ( 'NONE',  ( -0.3450121214752278065, 0.9385982292947087080, -0.000000000000000000 ) ) ;
#8190 = CARTESIAN_POINT ( 'NONE',  ( 48.01140435219951996, 98.06049967264873146, 35.83527830041809636 ) ) ;
#8191 = CARTESIAN_POINT ( 'NONE',  ( -151.4692556286852891, -196.9891397928655010, 39.65701158161630246 ) ) ;
#8192 = CARTESIAN_POINT ( 'NONE',  ( 39.42975644700377558, 84.41518717409400097, 36.81289934271958941 ) ) ;
#8193 = DIRECTION ( 'NONE',  ( 0.4683024526015100442, -0.8835682276357669229, 0.000000000000000000 ) ) ;
#8194 = CARTESIAN_POINT ( 'NONE',  ( 43.01140435219951996, 10.71049967264875491, 34.21067981925357060 ) ) ;
#8195 = ORIENTED_EDGE ( 'NONE', *, *, #1914, .F. ) ;
#8196 = CARTESIAN_POINT ( 'NONE',  ( 45.74753988029933538, 64.42977050742732104, 37.97664729208901946 ) ) ;
#8197 = CARTESIAN_POINT ( 'NONE',  ( -160.8964159109769696, -158.0438272943107165, 46.59394152635518793 ) ) ;
#8198 = CARTESIAN_POINT ( 'NONE',  ( 75.16956835342354282, 131.6452004531123805, 5.196376467030073165 ) ) ;
#8199 = CARTESIAN_POINT ( 'NONE',  ( -145.6429501568359797, -183.2084106276440423, 41.63779006702063867 ) ) ;
#8200 = ORIENTED_EDGE ( 'NONE', *, *, #5202, .T. ) ;
#8201 = CARTESIAN_POINT ( 'NONE',  ( 43.01140435219951286, 150.8651871740940180, 38.86567161673127657 ) ) ;
#8202 = CARTESIAN_POINT ( 'NONE',  ( -141.4692556286852891, -159.8391397928654669, 46.40781461928724383 ) ) ;
#8203 = CARTESIAN_POINT ( 'NONE',  ( 45.74753988029934249, 113.3297705074272983, 30.44471234641812174 ) ) ;
#8204 = CARTESIAN_POINT ( 'NONE',  ( 36.55618291757107841, 153.5264344809625641, -3.375052104409746789 ) ) ;
#8205 = ORIENTED_EDGE ( 'NONE', *, *, #10963, .F. ) ;
#8206 = CARTESIAN_POINT ( 'NONE',  ( 44.55648932407425633, 130.8844580088725706, 29.45539723777780239 ) ) ;
#8207 = ORIENTED_EDGE ( 'NONE', *, *, #2884, .F. ) ;
#8208 = CARTESIAN_POINT ( 'NONE',  ( 40.27526882409969033, 114.8297705074273125, 37.97664729208901946 ) ) ;
#8209 = DIRECTION ( 'NONE',  ( 0.000000000000000000, 0.000000000000000000, 1.000000000000000000 ) ) ;
#8210 = CARTESIAN_POINT ( 'NONE',  ( 44.37947211624943833, 85.27977050742731535, 38.42115945441014446 ) ) ;
#8211 = CARTESIAN_POINT ( 'NONE',  ( 41.64333658814960870, 158.5151871740940237, 30.00020018409699318 ) ) ;
#8212 = EDGE_CURVE ( 'NONE', #7175, #16530, #511, .T. ) ;
#8213 = CARTESIAN_POINT ( 'NONE',  ( 41.83190538388809188, 154.0406478741334126, 4.796127949319595629 ) ) ;
#8214 = DIRECTION ( 'NONE',  ( 1.000000000000000000, 0.000000000000000000, 0.000000000000000000 ) ) ;
#8215 = DIRECTION ( 'NONE',  ( 0.000000000000000000, 0.000000000000000000, 1.000000000000000000 ) ) ;
#8216 = LINE ( 'NONE', #21665, #10983 ) ;
#8217 = CARTESIAN_POINT ( 'NONE',  ( -151.4692556286852891, -180.2391397928654442, 39.14238933923362396 ) ) ;
#8218 = CARTESIAN_POINT ( 'NONE',  ( 38.01140435219952707, 156.7104996726487514, 34.21067981925357060 ) ) ;
#8219 = CARTESIAN_POINT ( 'NONE',  ( -151.4692556286852891, -193.1438272943107393, 59.56931450028537967 ) ) ;
#8220 = CARTESIAN_POINT ( 'NONE',  ( 38.01140435219952707, 125.7844580088725905, 34.21067981925357060 ) ) ;
#8221 = CARTESIAN_POINT ( 'NONE',  ( 40.27526882409969033, 98.92977050742732104, 30.44471234641811819 ) ) ;
#8222 = CARTESIAN_POINT ( 'NONE',  ( 20.52669235689029037, 137.0142703344444897, 22.89568392956547882 ) ) ;
#8223 = CARTESIAN_POINT ( 'NONE',  ( -160.8964159109769696, -179.0438272943107449, 46.59394152635518793 ) ) ;
#8224 = CARTESIAN_POINT ( 'NONE',  ( 43.01140435219951286, 86.36518717409400381, 29.55568802177586107 ) ) ;
#8225 = CARTESIAN_POINT ( 'NONE',  ( 43.01140435219951996, 10.71049967264875491, 34.21067981925357060 ) ) ;
#8226 = ORIENTED_EDGE ( 'NONE', *, *, #17669, .F. ) ;
#8227 = FACE_OUTER_BOUND ( 'NONE', #5689, .T. ) ;
#8228 = CARTESIAN_POINT ( 'NONE',  ( 65.27013532398795803, 145.9152199903044504, 11.62486143609835310 ) ) ;
#8229 = CARTESIAN_POINT ( 'NONE',  ( 45.74753988029934249, 145.4297705074273210, 37.97664729208901235 ) ) ;
#8230 = CARTESIAN_POINT ( 'NONE',  ( 15.11514590861459162, 123.4468881749472615, -3.696500957071167104 ) ) ;
#8231 = EDGE_CURVE ( 'NONE', #2768, #4323, #11182, .T. ) ;
#8232 = CARTESIAN_POINT ( 'NONE',  ( 41.64333658814960870, 66.97977050742731819, 38.42115945441014446 ) ) ;
#8233 = VERTEX_POINT ( 'NONE', #1382 ) ;
#8234 = CARTESIAN_POINT ( 'NONE',  ( 45.74753988029933538, 142.4297705074273495, 37.97664729208901946 ) ) ;
#8235 = CARTESIAN_POINT ( 'NONE',  ( 38.58424406990784661, 99.52977050742728693, 35.64915139335016647 ) ) ;
#8236 = DIRECTION ( 'NONE',  ( -0.000000000000000000, -0.000000000000000000, 1.000000000000000000 ) ) ;
#8237 = CARTESIAN_POINT ( 'NONE',  ( 44.55648932407425633, 109.6104996726487428, 38.96596240072933170 ) ) ;
#8238 = CARTESIAN_POINT ( 'NONE',  ( 40.27526882409969033, 68.66518717409400097, 30.44471234641811819 ) ) ;
#8239 = CARTESIAN_POINT ( 'NONE',  ( 43.01140435219957681, 96.53445800887259054, 39.21067981925356349 ) ) ;
#8240 = CARTESIAN_POINT ( 'NONE',  ( -157.2955611005345986, -157.4438272943107222, 57.67623309621197336 ) ) ;
#8241 = LINE ( 'NONE', #4930, #7947 ) ;
#8242 = CARTESIAN_POINT ( 'NONE',  ( -151.4692556286852891, -180.8130981290892976, 60.17163382399899518 ) ) ;
#8243 = CARTESIAN_POINT ( 'NONE',  ( 41.46631938032478359, 111.1104996726487428, 29.45539723777780239 ) ) ;
#8244 = CARTESIAN_POINT ( 'NONE',  ( 47.05648932407426344, 153.9844580088725934, 37.14960608071593384 ) ) ;
#8245 = CARTESIAN_POINT ( 'NONE',  ( 44.37947211624943833, 131.4797705074273040, 30.00020018409699318 ) ) ;
#8246 =( BOUNDED_CURVE ( )  B_SPLINE_CURVE ( 2, ( #5622, #7184, #15448, #17301, #8622, #5510, #233, #2000, #13781, #8842, #6971, #20411, #5307 ),
 .UNSPECIFIED., .F., .F. ) 
 B_SPLINE_CURVE_WITH_KNOTS ( ( 3, 2, 2, 2, 2, 2, 3 ),
 ( 0.8161764705882352811, 0.8176470588235293935, 0.8205882352941176183, 0.8235294117647058432, 0.8264705882352940680, 0.8294117647058824039, 0.8308823529411765163 ),
 .UNSPECIFIED. ) 
 CURVE ( )  GEOMETRIC_REPRESENTATION_ITEM ( )  RATIONAL_B_SPLINE_CURVE ( ( 0.9755282581475768211, 0.9755282581475768211, 1.000000000000000000, 0.9510565162951535312, 1.000000000000000000, 0.9510565162951535312, 1.000000000000000000, 0.9510565162951535312, 1.000000000000000000, 0.9510565162951535312, 1.000000000000000000, 0.9755282581475768211, 0.9755282581475768211 ) ) 
 REPRESENTATION_ITEM ( '' )  );
#8247 = CARTESIAN_POINT ( 'NONE',  ( 63.06653971011325410, 92.06373373134326243, 19.64449301269484849 ) ) ;
#8248 = CARTESIAN_POINT ( 'NONE',  ( 41.64333658814960870, 113.5151871740940095, 30.00020018409699318 ) ) ;
#8249 = DIRECTION ( 'NONE',  ( 0.000000000000000000, 0.000000000000000000, 1.000000000000000000 ) ) ;
#8250 = CARTESIAN_POINT ( 'NONE',  ( 43.01140435219951996, 10.71049967264875491, 39.21067981925356349 ) ) ;
#8251 = CARTESIAN_POINT ( 'NONE',  ( 52.81156257015842925, 87.19036605886009283, 8.010245892729333406 ) ) ;
#8252 = CARTESIAN_POINT ( 'NONE',  ( 15.53003795322992353, 126.2325256570730687, 2.418278830334454899 ) ) ;
#8253 = CARTESIAN_POINT ( 'NONE',  ( -141.4692556286852891, -155.9130981290893203, 46.40781461928724383 ) ) ;
#8254 = CARTESIAN_POINT ( 'NONE',  ( 40.27526882409969744, 99.82977050742731251, 37.97664729208901235 ) ) ;
#8255 = AXIS2_PLACEMENT_3D ( 'NONE', #16276, #7706, #2831 ) ;
#8256 = ORIENTED_EDGE ( 'NONE', *, *, #593, .F. ) ;
#8257 = ADVANCED_FACE ( 'NONE', ( #14714 ), #15043, .F. ) ;
#8258 = CARTESIAN_POINT ( 'NONE',  ( 43.80332655382219542, 145.9575765865523067, 29.21067981925356705 ) ) ;
#8259 = ORIENTED_EDGE ( 'NONE', *, *, #11008, .F. ) ;
#8260 = CARTESIAN_POINT ( 'NONE',  ( 47.05648932407426344, 82.58445800887258770, 31.27175355779120025 ) ) ;
#8261 = CARTESIAN_POINT ( 'NONE',  ( 39.92123440845005433, 86.33445800887258770, 29.95742577749336988 ) ) ;
#8262 = CARTESIAN_POINT ( 'NONE',  ( 39.92123440845004723, 135.2604996726487343, 29.95742577749337343 ) ) ;
#8264 = CARTESIAN_POINT ( 'NONE',  ( 69.89089498905519804, 111.6491328518190613, -0.005813817042542732995 ) ) ;
#8263 = CARTESIAN_POINT ( 'NONE',  ( 40.27526882409969033, 95.66518717409398675, 30.44471234641811819 ) ) ;
#8265 = EDGE_CURVE ( 'NONE', #1696, #11702, #633, .T. ) ;
#8266 = CARTESIAN_POINT ( 'NONE',  ( -160.8964159109769696, -164.0084106276440536, 52.72008163687743121 ) ) ;
#8267 = CARTESIAN_POINT ( 'NONE',  ( -142.0420953463935803, -186.5438272943107449, 52.72008163687743831 ) ) ;
#8269 = CARTESIAN_POINT ( 'NONE',  ( 48.01140435219951996, 70.28445800887257633, 34.21067981925357060 ) ) ;
#8268 = CARTESIAN_POINT ( 'NONE',  ( -154.5594255724347761, -165.9630981290893033, 59.16757674456785310 ) ) ;
#8270 = CARTESIAN_POINT ( 'NONE',  ( -138.5468111011521160, 759.4679229819337252, -0.8325491102011938205 ) ) ;
#8271 = CARTESIAN_POINT ( 'NONE',  ( -148.3790856849358306, -176.4630981290893033, 40.14644641866477315 ) ) ;
#8272 = CARTESIAN_POINT ( 'NONE',  ( 44.55648932407425633, 114.6844580088725820, 38.96596240072933170 ) ) ;
#8273 = CARTESIAN_POINT ( 'NONE',  ( 40.27526882409969033, 63.56518717409399954, 37.97664729208901946 ) ) ;
#8274 = CARTESIAN_POINT ( 'NONE',  ( 43.01140435219951996, 10.71049967264875491, 39.21067981925356349 ) ) ;
#8275 = CARTESIAN_POINT ( 'NONE',  ( 14.88286428391304561, 100.3963227437532595, 8.410691821786379307 ) ) ;
#8276 = CARTESIAN_POINT ( 'NONE',  ( 38.58424406990785371, 146.9651871740940123, 32.77220824515697473 ) ) ;
#8277 = CARTESIAN_POINT ( 'NONE',  ( -151.4692556286852891, -157.1438272943107393, 59.56931450028537967 ) ) ;
#8278 = CARTESIAN_POINT ( 'NONE',  ( -143.8425227516148084, -171.3584106276440764, 44.11586579668791330 ) ) ;
#8279 = VERTEX_POINT ( 'NONE', #19680 ) ;
#8280 = CARTESIAN_POINT ( 'NONE',  ( 45.22504609509771001, 59.11591859955431971, 30.37668211462113277 ) ) ;
#8281 = CARTESIAN_POINT ( 'NONE',  ( -142.0420953463936087, -162.6584106276440593, 49.65701158161630957 ) ) ;
#8282 = CARTESIAN_POINT ( 'NONE',  ( 15.77498628565902727, 140.7233915340666499, 22.81684008552556975 ) ) ;
#8283 = CARTESIAN_POINT ( 'NONE',  ( 44.55648932407425633, 111.6844580088725820, 38.96596240072933170 ) ) ;
#8284 = CARTESIAN_POINT ( 'NONE',  ( 47.43856463449117200, 127.7651871740940237, 32.77220824515698183 ) ) ;
#8285 = CARTESIAN_POINT ( 'NONE',  ( 8.987667018801221985, 116.9306527918008527, -4.013769077970609445 ) ) ;
#8286 = VERTEX_POINT ( 'NONE', #8007 ) ;
#8287 = ORIENTED_EDGE ( 'NONE', *, *, #9209, .T. ) ;
#8288 = ORIENTED_EDGE ( 'NONE', *, *, #18616, .F. ) ;
#8289 = CARTESIAN_POINT ( 'NONE',  ( 41.64333658814960870, 153.9797705074273324, 38.42115945441014446 ) ) ;
#8291 = CARTESIAN_POINT ( 'NONE',  ( 33.01799438418878907, 146.2770090272405810, 10.51364782838779099 ) ) ;
#8290 = CARTESIAN_POINT ( 'NONE',  ( 41.64333658814960870, 122.5151871740940095, 30.00020018409699318 ) ) ;
#8292 = EDGE_CURVE ( 'NONE', #7116, #5296, #20131, .T. ) ;
#8293 = CARTESIAN_POINT ( 'NONE',  ( 43.01140435219951286, 77.96049967264873715, 28.95336869806222779 ) ) ;
#8294 = LINE ( 'NONE', #20096, #15341 ) ;
#8295 = AXIS2_PLACEMENT_3D ( 'NONE', #16819, #13520, #20574 ) ;
#8296 = CARTESIAN_POINT ( 'NONE',  ( -148.3790856849358306, -170.4630981290893033, 40.14644641866477315 ) ) ;
#8297 = CARTESIAN_POINT ( 'NONE',  ( -97.23064952102208736, 13.78046159333444720, -19.99999999999997868 ) ) ;
#8298 = CARTESIAN_POINT ( 'NONE',  ( 43.01140435219951286, 89.36518717409398960, 29.55568802177586463 ) ) ;
#8299 = CARTESIAN_POINT ( 'NONE',  ( 42.21948215057684450, 82.38361825032845331, 39.21067981925355639 ) ) ;
#8300 = CARTESIAN_POINT ( 'NONE',  ( -151.4692556286852891, -196.9891397928655010, 49.65701158161630957 ) ) ;
#8301 = VERTEX_POINT ( 'NONE', #9552 ) ;
#8302 = CARTESIAN_POINT ( 'NONE',  ( 47.43856463449118621, 61.87977050742732388, 34.21067981925357060 ) ) ;
#8303 = CARTESIAN_POINT ( 'NONE',  ( -160.8964159109769696, -185.0084106276440821, 52.72008163687743121 ) ) ;
#8304 = CARTESIAN_POINT ( 'NONE',  ( 35.69068542950036260, 86.46542255174357194, 7.577194441455407770 ) ) ;
#8305 = CARTESIAN_POINT ( 'NONE',  ( -151.4692556286852891, -188.9084106276440593, 39.74470866294723947 ) ) ;
#8306 = ORIENTED_EDGE ( 'NONE', *, *, #12097, .F. ) ;
#8307 = APPLICATION_CONTEXT ( 'automotive_design' ) ;
#8308 = CARTESIAN_POINT ( 'NONE',  ( 45.74753988029933538, 149.0651871740940067, 30.44471234641811819 ) ) ;
#8309 = CARTESIAN_POINT ( 'NONE',  ( 43.01140435219951996, 154.4604996726487798, 39.21067981925357060 ) ) ;
#8310 = CARTESIAN_POINT ( 'NONE',  ( 47.43856463449117911, 112.7297705074273324, 35.64915139335015937 ) ) ;
#8311 = CARTESIAN_POINT ( 'NONE',  ( 48.01140435219951996, 154.1344580088725991, 35.83527830041809636 ) ) ;
#8312 = EDGE_LOOP ( 'NONE', ( #4251, #4074 ) ) ;
#8313 = AXIS2_PLACEMENT_3D ( 'NONE', #10086, #15374, #3686 ) ;
#8314 = ADVANCED_FACE ( 'NONE', ( #1495 ), #4572, .T. ) ;
#8315 = CARTESIAN_POINT ( 'NONE',  ( 22.17150742865759483, 138.9041494244890771, -4.010207742755246052 ) ) ;
#8316 = VERTEX_POINT ( 'NONE', #13175 ) ;
#8317 = CARTESIAN_POINT ( 'NONE',  ( 44.37947211624943833, 118.2797705074273296, 38.42115945441014446 ) ) ;
#8318 = DIRECTION ( 'NONE',  ( -0.9385982292947087080, -0.3450121214752276955, -0.000000000000000000 ) ) ;
#8319 = CARTESIAN_POINT ( 'NONE',  ( 41.64333658814960870, 153.7151871740940123, 38.42115945441014446 ) ) ;
#8320 = CARTESIAN_POINT ( 'NONE',  ( 52.81156257015842925, 87.19036605886009283, 8.010245892729333406 ) ) ;
#8321 = CARTESIAN_POINT ( 'NONE',  ( 43.01140435219951286, 119.9604996726487229, 29.21067981925356705 ) ) ;
#8322 = CARTESIAN_POINT ( 'NONE',  ( 164.7397274782390184, 67.46000011932014218, 14.00000000000001776 ) ) ;
#8323 = FACE_OUTER_BOUND ( 'NONE', #7519, .T. ) ;
#8324 = CARTESIAN_POINT ( 'NONE',  ( -159.5594255724347761, -176.1891397928654612, 55.53486410454104316 ) ) ;
#8325 = DIRECTION ( 'NONE',  ( 0.000000000000000000, 1.000000000000000000, 0.000000000000000000 ) ) ;
#8326 = DIRECTION ( 'NONE',  ( 0.000000000000000000, 1.000000000000000000, 0.000000000000000000 ) ) ;
#8327 = CARTESIAN_POINT ( 'NONE',  ( -39.63192160874135084, -136.9891397928655010, 20.00000000000002132 ) ) ;
#8328 = VECTOR ( 'NONE', #15622, 1000.000000000000000 ) ;
#8329 = CARTESIAN_POINT ( 'NONE',  ( 45.74753988029933538, 95.32977050742729830, 30.44471234641811819 ) ) ;
#8330 = CARTESIAN_POINT ( 'NONE',  ( 25.76509531087978289, 97.49384569152056201, 21.15186415193267067 ) ) ;
#8331 = CARTESIAN_POINT ( 'NONE',  ( -160.8964159109769696, -187.7438272943107336, 52.72008163687743121 ) ) ;
#8332 = CARTESIAN_POINT ( 'NONE',  ( 39.42975644700377558, 89.81518717409400665, 31.60846029578754468 ) ) ;
#8333 = DIRECTION ( 'NONE',  ( 0.9393725726208708160, 0.3428981916074316794, -0.000000000000000000 ) ) ;
#8334 = ORIENTED_EDGE ( 'NONE', *, *, #20907, .F. ) ;
#8335 = CARTESIAN_POINT ( 'NONE',  ( -124.3720331620955619, 13.78046159333444720, 4.000000000000021316 ) ) ;
#8336 = CARTESIAN_POINT ( 'NONE',  ( 38.58424406990785371, 141.5297705074272869, 35.64915139335015937 ) ) ;
#8337 = CARTESIAN_POINT ( 'NONE',  ( 21.63557314705429846, 101.6375443364048152, 2.375099401820868206 ) ) ;
#8338 = EDGE_CURVE ( 'NONE', #3067, #20247, #4794, .T. ) ;
#8339 = DIRECTION ( 'NONE',  ( -0.000000000000000000, -0.000000000000000000, -1.000000000000000000 ) ) ;
#8340 = VERTEX_POINT ( 'NONE', #18015 ) ;
#8341 = AXIS2_PLACEMENT_3D ( 'NONE', #10816, #21167, #15973 ) ;
#8342 = CARTESIAN_POINT ( 'NONE',  ( 47.43856463449117200, 142.7297705074273324, 35.64915139335016647 ) ) ;
#8343 = CARTESIAN_POINT ( 'NONE',  ( 40.27526882409969033, 95.92977050742732104, 30.44471234641811819 ) ) ;
#8344 = AXIS2_PLACEMENT_3D ( 'NONE', #10960, #496, #9208 ) ;
#8345 = CARTESIAN_POINT ( 'NONE',  ( -159.5594255724347761, -193.2630981290893146, 55.53486410454104316 ) ) ;
#8346 = CARTESIAN_POINT ( 'NONE',  ( 39.92123440845004723, 115.1604996726487542, 38.46393386101376421 ) ) ;
#8347 = CARTESIAN_POINT ( 'NONE',  ( 39.42975644700377558, 66.41518717409400097, 36.81289934271958941 ) ) ;
#8348 = CARTESIAN_POINT ( 'NONE',  ( 43.01140435219951286, 146.0344580088725479, 29.21067981925356705 ) ) ;
#8349 = CARTESIAN_POINT ( 'NONE',  ( -160.8964159109769696, -163.8938272943107393, 49.65701158161630957 ) ) ;
#8350 = DIRECTION ( 'NONE',  ( 0.000000000000000000, 0.000000000000000000, -1.000000000000000000 ) ) ;
#8351 = CARTESIAN_POINT ( 'NONE',  ( -145.2889157411863721, -177.5130981290893430, 58.16351966513671812 ) ) ;
#8352 = CARTESIAN_POINT ( 'NONE',  ( 38.96631938032478359, 111.4104996726487400, 31.27175355779120025 ) ) ;
#8353 = CARTESIAN_POINT ( 'NONE',  ( 38.96631938032478359, 152.4844580088725934, 31.27175355779120025 ) ) ;
#8354 = CARTESIAN_POINT ( 'NONE',  ( 40.27526882409969033, 122.9297705074272926, 30.44471234641811819 ) ) ;
#8355 = CARTESIAN_POINT ( 'NONE',  ( 53.94306145151312393, 87.38125778962682944, 12.97772928308168616 ) ) ;
#8356 = CYLINDRICAL_SURFACE ( 'NONE', #7128, 4.999999999999997335 ) ;
#8357 = AXIS2_PLACEMENT_3D ( 'NONE', #12124, #15762, #3979 ) ;
#8358 = CARTESIAN_POINT ( 'NONE',  ( 40.27526882409969744, 119.6651871740940010, 30.44471234641812174 ) ) ;
#8359 = CARTESIAN_POINT ( 'NONE',  ( -151.4692556286852607, -166.7391397928654158, 59.65701158161632378 ) ) ;
#8360 = CARTESIAN_POINT ( 'NONE',  ( 43.01140435219951996, 10.71049967264875491, 34.21067981925357060 ) ) ;
#8361 = CARTESIAN_POINT ( 'NONE',  ( 45.50561661668613311, 153.9697812235645245, 4.915054502968218664 ) ) ;
#8362 = CARTESIAN_POINT ( 'NONE',  ( 31.84750084766683287, 94.01163676417708359, 0.8705387173494113506 ) ) ;
#8363 = CARTESIAN_POINT ( 'NONE',  ( 151.4773229304660731, 84.89323405393692212, 14.00000000000001776 ) ) ;
#8364 = CARTESIAN_POINT ( 'NONE',  ( 45.74753988029934249, 95.32977050742729830, 30.44471234641812174 ) ) ;
#8365 = ORIENTED_EDGE ( 'NONE', *, *, #14042, .F. ) ;
#8366 = VECTOR ( 'NONE', #10639, 1000.000000000000000 ) ;
#8367 = CARTESIAN_POINT ( 'NONE',  ( 157.5268905834513475, 193.0332408774651185, -44.99999999999997158 ) ) ;
#8368 = VERTEX_POINT ( 'NONE', #11515 ) ;
#8369 = CARTESIAN_POINT ( 'NONE',  ( 47.05648932407426344, 70.58445800887257349, 31.27175355779120025 ) ) ;
#8370 = CARTESIAN_POINT ( 'NONE',  ( 72.34521997529867576, 314.8592298662555322, -4.000000000000003553 ) ) ;
#8371 = AXIS2_PLACEMENT_3D ( 'NONE', #13916, #13812, #20550 ) ;
#8372 = CARTESIAN_POINT ( 'NONE',  ( 43.01140435219951286, 140.9604996726487514, 28.95336869806222779 ) ) ;
#8374 = CARTESIAN_POINT ( 'NONE',  ( 16.71508173162657229, 129.8698440624217483, 3.565528294796503683 ) ) ;
#8373 = CARTESIAN_POINT ( 'NONE',  ( 45.74753988029933538, 95.06518717409400665, 30.44471234641811819 ) ) ;
#8375 =( BOUNDED_CURVE ( )  B_SPLINE_CURVE ( 2, ( #16363, #4352, #6116, #11190, #13177, #1384, #1275, #19909, #14495, #12739, #2816, #1166, #3148 ),
 .UNSPECIFIED., .F., .F. ) 
 B_SPLINE_CURVE_WITH_KNOTS ( ( 3, 2, 2, 2, 2, 2, 3 ),
 ( 0.3014705882352941013, 0.3029411764705882137, 0.3058823529411764941, 0.3088235294117647189, 0.3117647058823529438, 0.3147058823529411686, 0.3161764705882352811 ),
 .UNSPECIFIED. ) 
 CURVE ( )  GEOMETRIC_REPRESENTATION_ITEM ( )  RATIONAL_B_SPLINE_CURVE ( ( 0.9755282581475768211, 0.9755282581475768211, 1.000000000000000000, 0.9510565162951535312, 1.000000000000000000, 0.9510565162951535312, 1.000000000000000000, 0.9510565162951535312, 1.000000000000000000, 0.9510565162951535312, 1.000000000000000000, 0.9755282581475768211, 0.9755282581475768211 ) ) 
 REPRESENTATION_ITEM ( '' )  );
#8376 = CARTESIAN_POINT ( 'NONE',  ( -142.0420953463935803, -168.5084106276440536, 46.59394152635518793 ) ) ;
#8377 = CARTESIAN_POINT ( 'NONE',  ( -157.2955611005345986, -190.4438272943107222, 57.67623309621197336 ) ) ;
#8379 = FACE_OUTER_BOUND ( 'NONE', #4760, .T. ) ;
#8378 = DIRECTION ( 'NONE',  ( 0.000000000000000000, 0.000000000000000000, -1.000000000000000000 ) ) ;
#8380 = PLANE ( 'NONE',  #11227 ) ;
#8381 = DIRECTION ( 'NONE',  ( 0.000000000000000000, -1.000000000000000000, 0.000000000000000000 ) ) ;
#8382 = CARTESIAN_POINT ( 'NONE',  ( 43.01140435219951286, 80.96049967264873715, 29.21067981925356705 ) ) ;
#8383 = CARTESIAN_POINT ( 'NONE',  ( 39.42975644700377558, 147.6797705074273495, 36.81289934271958941 ) ) ;
#8384 = CARTESIAN_POINT ( 'NONE',  ( 43.01140435219951996, 10.71049967264875491, 39.21067981925356349 ) ) ;
#8385 = CARTESIAN_POINT ( 'NONE',  ( 63.41425016244589585, 92.41789933959738335, 6.624947895572852019 ) ) ;
#8386 = CARTESIAN_POINT ( 'NONE',  ( 45.74753988029934249, 145.1651871740940010, 37.97664729208901235 ) ) ;
#8387 = CARTESIAN_POINT ( 'NONE',  ( -143.8425227516148084, -162.0938272943107279, 44.11586579668791330 ) ) ;
#8388 = CARTESIAN_POINT ( 'NONE',  ( -143.8425227516148084, -174.3584106276440480, 44.11586579668791330 ) ) ;
#8389 = ORIENTED_EDGE ( 'NONE', *, *, #21084, .F. ) ;
#8390 = CARTESIAN_POINT ( 'NONE',  ( 40.27526882409969744, 60.56518717409398533, 37.97664729208901235 ) ) ;
#8391 = CARTESIAN_POINT ( 'NONE',  ( -160.8964159109769696, -158.0084106276440536, 52.72008163687743121 ) ) ;
#8392 = CARTESIAN_POINT ( 'NONE',  ( 68.00896726847550156, 133.1338957242411709, 4.128172222816925085 ) ) ;
#8393 = CIRCLE ( 'NONE', #21765, 21.47274291077713571 ) ;
#8394 = FILL_AREA_STYLE_COLOUR ( '', #17614 ) ;
#8395 = CARTESIAN_POINT ( 'NONE',  ( 44.37947211624943833, 125.2151871740939981, 30.00020018409699318 ) ) ;
#8396 = ORIENTED_EDGE ( 'NONE', *, *, #11473, .T. ) ;
#8397 = VERTEX_POINT ( 'NONE', #21674 ) ;
#8398 = CARTESIAN_POINT ( 'NONE',  ( 39.92123440845005433, 113.3344580088725735, 29.95742577749336988 ) ) ;
#8399 = EDGE_CURVE ( 'NONE', #2386, #18846, #11293, .T. ) ;
#8400 = ORIENTED_EDGE ( 'NONE', *, *, #2211, .T. ) ;
#8401 = CARTESIAN_POINT ( 'NONE',  ( 38.01140435219951996, 107.6344580088725706, 32.58608133808903773 ) ) ;
#8402 = CARTESIAN_POINT ( 'NONE',  ( 39.42975644700377558, 153.0797705074273267, 31.60846029578754468 ) ) ;
#8403 = CARTESIAN_POINT ( 'NONE',  ( 39.42975644700377558, 69.07977050742732672, 31.60846029578754468 ) ) ;
#8405 = CARTESIAN_POINT ( 'NONE',  ( 41.25620118372704326, 148.0523446076144580, 3.846850258842608117 ) ) ;
#8404 = CARTESIAN_POINT ( 'NONE',  ( 40.27526882409969033, 126.5651871740940209, 37.97664729208901946 ) ) ;
#8406 = CARTESIAN_POINT ( 'NONE',  ( 47.05648932407426344, 86.51049967264874851, 31.27175355779120025 ) ) ;
#8407 = DIRECTION ( 'NONE',  ( -0.000000000000000000, 1.000000000000000000, -0.000000000000000000 ) ) ;
#8408 = CARTESIAN_POINT ( 'NONE',  ( 156.5548063637509415, 177.1359029563629406, -44.99999999999997158 ) ) ;
#8409 = LINE ( 'NONE', #4756, #7287 ) ;
#8410 = CARTESIAN_POINT ( 'NONE',  ( 45.74753988029933538, 79.16518717409398675, 37.97664729208901946 ) ) ;
#8411 = PRODUCT_DEFINITION_CONTEXT ( 'detailed design', #12800, 'design' ) ;
#8412 = CARTESIAN_POINT ( 'NONE',  ( 38.01140435219952707, 81.56049967264873146, 32.58608133808903773 ) ) ;
#8413 = DIRECTION ( 'NONE',  ( -0.000000000000000000, 0.000000000000000000, -1.000000000000000000 ) ) ;
#8414 = ORIENTED_EDGE ( 'NONE', *, *, #21322, .F. ) ;
#8415 = CARTESIAN_POINT ( 'NONE',  ( 38.58424406990786082, 63.37977050742732388, 34.21067981925357060 ) ) ;
#8416 = CARTESIAN_POINT ( 'NONE',  ( -145.6429501568359797, -186.2084106276440707, 41.63779006702063867 ) ) ;
#8417 = CARTESIAN_POINT ( 'NONE',  ( 15.97061701817242785, 140.8453463817331794, 16.82122940411608170 ) ) ;
#8418 = CARTESIAN_POINT ( 'NONE',  ( -151.4692556286852891, -179.9084106276440593, 39.74470866294723947 ) ) ;
#8419 = ORIENTED_EDGE ( 'NONE', *, *, #5300, .T. ) ;
#8420 = CARTESIAN_POINT ( 'NONE',  ( 40.27526882409969033, 152.6651871740940010, 30.44471234641811819 ) ) ;
#8421 = ADVANCED_FACE ( 'NONE', ( #9661 ), #16361, .T. ) ;
#8422 = CARTESIAN_POINT ( 'NONE',  ( 157.5268905834513475, 193.0332408774651185, 14.00000000000001776 ) ) ;
#8423 = EDGE_CURVE ( 'NONE', #6176, #15753, #4685, .T. ) ;
#8424 = CARTESIAN_POINT ( 'NONE',  ( 40.27526882409969744, 110.9297705074273068, 30.44471234641812174 ) ) ;
#8425 = CARTESIAN_POINT ( 'NONE',  ( 20.75180444880664510, 93.89949152720284076, -5.875022464008872625 ) ) ;
#8426 = ORIENTED_EDGE ( 'NONE', *, *, #7072, .F. ) ;
#8427 = CARTESIAN_POINT ( 'NONE',  ( 14.81332417359726783, 119.6334487847019403, -4.843746996953559147 ) ) ;
#8428 = VERTEX_POINT ( 'NONE', #3034 ) ;
#8429 = CARTESIAN_POINT ( 'NONE',  ( 47.43856463449117200, 121.7297705074273040, 35.64915139335016647 ) ) ;
#8430 = ADVANCED_FACE ( 'NONE', ( #9772 ), #16468, .T. ) ;
#8431 = DIRECTION ( 'NONE',  ( 0.000000000000000000, 0.000000000000000000, 1.000000000000000000 ) ) ;
#8432 = CARTESIAN_POINT ( 'NONE',  ( 43.01140435219951286, 150.8651871740940180, 38.86567161673127657 ) ) ;
#8433 = CARTESIAN_POINT ( 'NONE',  ( 70.43474449472395804, 99.54920534645194152, 7.295875980836476593 ) ) ;
#8434 = CARTESIAN_POINT ( 'NONE',  ( -81.61981105773979550, 604.5992151483073940, -23.16745088979876499 ) ) ;
#8435 = DIRECTION ( 'NONE',  ( 0.000000000000000000, -1.000000000000000000, 0.000000000000000000 ) ) ;
#8436 = CARTESIAN_POINT ( 'NONE',  ( -145.2889157411863721, -178.4391397928654044, 58.16351966513671812 ) ) ;
#8437 = CARTESIAN_POINT ( 'NONE',  ( 162.3411339277076308, 184.7625696037766261, -19.99999999999997868 ) ) ;
#8438 = UNCERTAINTY_MEASURE_WITH_UNIT (LENGTH_MEASURE( 1.000000000000000082E-05 ), #21622, 'distance_accuracy_value', 'NONE');
#8439 = DIRECTION ( 'NONE',  ( 0.3450121214752276955, -0.9385982292947087080, 0.000000000000000000 ) ) ;
#8440 = DIRECTION ( 'NONE',  ( 0.5061580162706794672, 0.8624407588727069918, 0.000000000000000000 ) ) ;
#8442 = AXIS2_PLACEMENT_3D ( 'NONE', #1537, #14862, #11666 ) ;
#8441 = CONTEXT_DEPENDENT_SHAPE_REPRESENTATION ( #8595, #19254 ) ;
#8443 = EDGE_CURVE ( 'NONE', #2592, #20087, #9876, .T. ) ;
#8444 = VECTOR ( 'NONE', #14827, 1000.000000000000000 ) ;
#8445 = CARTESIAN_POINT ( 'NONE',  ( 39.42975644700377558, 90.67977050742732104, 36.81289934271958941 ) ) ;
#8446 =( BOUNDED_CURVE ( )  B_SPLINE_CURVE ( 2, ( #5059, #15417, #11773, #10023, #13327, #13641, #20271, #313, #20487, #15306, #10242, #5377, #14961 ),
 .UNSPECIFIED., .F., .F. ) 
 B_SPLINE_CURVE_WITH_KNOTS ( ( 3, 2, 2, 2, 2, 2, 3 ),
 ( 0.9632352941176470784, 0.9647058823529411908, 0.9676470588235294157, 0.9705882352941176405, 0.9735294117647058654, 0.9764705882352940902, 0.9779411764705882026 ),
 .UNSPECIFIED. ) 
 CURVE ( )  GEOMETRIC_REPRESENTATION_ITEM ( )  RATIONAL_B_SPLINE_CURVE ( ( 0.9755282581475768211, 0.9755282581475768211, 1.000000000000000000, 0.9510565162951535312, 1.000000000000000000, 0.9510565162951535312, 1.000000000000000000, 0.9510565162951535312, 1.000000000000000000, 0.9510565162951535312, 1.000000000000000000, 0.9755282581475768211, 0.9755282581475768211 ) ) 
 REPRESENTATION_ITEM ( '' )  );
#8447 = CARTESIAN_POINT ( 'NONE',  ( 14.94677925004173957, 122.6663546818147381, -4.724578312614759135 ) ) ;
#8448 = CARTESIAN_POINT ( 'NONE',  ( -159.0959885057557983, -170.1938272943107222, 44.11586579668791330 ) ) ;
#8449 = CARTESIAN_POINT ( 'NONE',  ( 44.37947211624943833, 89.21518717409399812, 30.00020018409699318 ) ) ;
#8450 = CARTESIAN_POINT ( 'NONE',  ( -130.4480969619998234, -136.9891397928655010, 67.64809332337415526 ) ) ;
#8451 = ORIENTED_EDGE ( 'NONE', *, *, #8292, .T. ) ;
#8452 = CARTESIAN_POINT ( 'NONE',  ( 43.01140435219951996, 119.9070776186055838, -19.99999999999997868 ) ) ;
#8453 = EDGE_CURVE ( 'NONE', #15661, #10393, #3484, .T. ) ;
#8454 = CARTESIAN_POINT ( 'NONE',  ( 30.18028515090226449, 151.2280014487717779, 17.43780275515692679 ) ) ;
#8455 = CARTESIAN_POINT ( 'NONE',  ( 46.59305225739526435, 143.1797705074273210, 31.60846029578754468 ) ) ;
#8456 = CARTESIAN_POINT ( 'NONE',  ( 24.14732448757077776, 99.05405632904258084, -4.767757741039170938 ) ) ;
#8457 = CARTESIAN_POINT ( 'NONE',  ( 38.01140435219952707, 119.7844580088725763, 34.21067981925357060 ) ) ;
#8458 = VERTEX_POINT ( 'NONE', #10095 ) ;
#8459 = CARTESIAN_POINT ( 'NONE',  ( 43.01140435219951286, 142.1297705074273097, 38.86567161673127657 ) ) ;
#8460 = AXIS2_PLACEMENT_3D ( 'NONE', #15525, #15839, #8706 ) ;
#8461 = CARTESIAN_POINT ( 'NONE',  ( 45.74753988029933538, 94.42977050742732104, 37.97664729208901946 ) ) ;
#8462 = LINE ( 'NONE', #16703, #6699 ) ;
#8463 = CARTESIAN_POINT ( 'NONE',  ( 39.42975644700377558, 59.81518717409399244, 31.60846029578754468 ) ) ;
#8464 = CARTESIAN_POINT ( 'NONE',  ( -154.5594255724347761, -170.1630981290893203, 40.14644641866476604 ) ) ;
#8465 = CARTESIAN_POINT ( 'NONE',  ( -154.3824083646099439, -163.2938272943107449, 58.62277379824867296 ) ) ;
#8466 = CARTESIAN_POINT ( 'NONE',  ( 39.92123440845005433, 109.1604996726487400, 38.46393386101375711 ) ) ;
#8467 = CARTESIAN_POINT ( 'NONE',  ( -151.4692556286852891, -167.3130981290893260, 39.14238933923362396 ) ) ;
#8468 = CARTESIAN_POINT ( 'NONE',  ( 38.01140435219952707, 111.5604996726487457, 32.58608133808903773 ) ) ;
#8469 = CARTESIAN_POINT ( 'NONE',  ( 43.01140435219951286, 143.0344580088726048, 28.95336869806222779 ) ) ;
#8470 = CARTESIAN_POINT ( 'NONE',  ( 43.01140435219951286, 122.6297705074273239, 29.55568802177586463 ) ) ;
#8471 = CARTESIAN_POINT ( 'NONE',  ( 65.22477088018504787, 102.4029861919955948, -1.586113490162427864 ) ) ;
#8472 = CARTESIAN_POINT ( 'NONE',  ( -151.4692556286852607, -184.7391397928654726, 59.65701158161632378 ) ) ;
#8473 = CARTESIAN_POINT ( 'NONE',  ( 38.58424406990785371, 120.2651871740939953, 35.64915139335015937 ) ) ;
#8474 = CARTESIAN_POINT ( 'NONE',  ( 129.5727795705175822, 84.89323405393692212, 14.00000000000001776 ) ) ;
#8475 = CLOSED_SHELL ( 'NONE', ( #9761, #18925, #8585, #13380, #6390, #3678, #966, #17842, #16477, #10699, #12632, #10454 ) ) ;
#8476 = AXIS2_PLACEMENT_3D ( 'NONE', #12078, #17144, #7136 ) ;
#8477 = CARTESIAN_POINT ( 'NONE',  ( 126.8576204525573274, -126.9891397928655010, 67.64809332337412684 ) ) ;
#8478 = CARTESIAN_POINT ( 'NONE',  ( 14.34121205894687456, 138.4663445754194697, 3.724531598165178092 ) ) ;
#8479 = CARTESIAN_POINT ( 'NONE',  ( 16.33471683235446292, 110.7640000046674089, -5.200637885961103102 ) ) ;
#8480 = DIRECTION ( 'NONE',  ( 0.000000000000000000, 0.000000000000000000, -1.000000000000000000 ) ) ;
#8481 = CARTESIAN_POINT ( 'NONE',  ( 44.37947211624943833, 85.27977050742731535, 38.42115945441014446 ) ) ;
#8482 = ORIENTED_EDGE ( 'NONE', *, *, #14487, .F. ) ;
#8483 = CARTESIAN_POINT ( 'NONE',  ( 43.01140435219951996, 119.9070776186055838, 50.00000000000002842 ) ) ;
#8484 = CARTESIAN_POINT ( 'NONE',  ( 47.05648932407426344, 73.58445800887257349, 31.27175355779120025 ) ) ;
#8485 = LINE ( 'NONE', #18612, #11937 ) ;
#8486 = VECTOR ( 'NONE', #15328, 1000.000000000000000 ) ;
#8487 = CARTESIAN_POINT ( 'NONE',  ( 41.46631938032478359, 132.1104996726487286, 29.45539723777780239 ) ) ;
#8489 = CARTESIAN_POINT ( 'NONE',  ( 19.07518309319397432, 143.9976739860571229, -17.03742665657317801 ) ) ;
#8488 = CARTESIAN_POINT ( 'NONE',  ( 44.37947211624943833, 85.01518717409399528, 38.42115945441014446 ) ) ;
#8490 = CARTESIAN_POINT ( 'NONE',  ( -154.3824083646099439, -161.7584106276440252, 40.69124936498395328 ) ) ;
#8491 = CARTESIAN_POINT ( 'NONE',  ( -145.6429501568359797, -188.9438272943106938, 41.63779006702063867 ) ) ;
#8492 = CARTESIAN_POINT ( 'NONE',  ( 39.92123440845005433, 93.26049967264872009, 29.95742577749336988 ) ) ;
#8493 = CARTESIAN_POINT ( 'NONE',  ( 47.05648932407426344, 126.9844580088725934, 37.14960608071593384 ) ) ;
#8494 = DIRECTION ( 'NONE',  ( 0.3450121214752279175, -0.9385982292947087080, -0.000000000000000000 ) ) ;
#8495 = CARTESIAN_POINT ( 'NONE',  ( 39.42975644700377558, 150.0797705074273267, 31.60846029578754468 ) ) ;
#8496 = CARTESIAN_POINT ( 'NONE',  ( 43.80332655382220963, 157.5373810949690494, 39.21067981925355639 ) ) ;
#8497 = CARTESIAN_POINT ( 'NONE',  ( 51.78234217841457365, 152.9971814535558963, 4.124977536042813142 ) ) ;
#8498 = CARTESIAN_POINT ( 'NONE',  ( 39.42975644700377558, 143.8151871740940067, 31.60846029578754468 ) ) ;
#8499 = CARTESIAN_POINT ( 'NONE',  ( -160.8964159109769696, -163.7438272943107336, 52.72008163687743121 ) ) ;
#8500 = CARTESIAN_POINT ( 'NONE',  ( -157.2955611005345986, -170.6084106276440480, 41.63779006702063867 ) ) ;
#8501 = ORIENTED_EDGE ( 'NONE', *, *, #19283, .T. ) ;
#8502 = CARTESIAN_POINT ( 'NONE',  ( 43.01140435219951286, 59.36518717409399670, 29.55568802177586107 ) ) ;
#8503 = CARTESIAN_POINT ( 'NONE',  ( -154.3824083646099439, -161.7584106276440252, 40.69124936498395328 ) ) ;
#8504 = CARTESIAN_POINT ( 'NONE',  ( 69.60802376816022274, 110.2920722108499518, -1.943010761821444943 ) ) ;
#8505 = FILL_AREA_STYLE ('',( #6 ) ) ;
#8506 = CARTESIAN_POINT ( 'NONE',  ( 46.59305225739526435, 124.9151871740940010, 31.60846029578754468 ) ) ;
#8507 = ORIENTED_EDGE ( 'NONE', *, *, #2211, .F. ) ;
#8508 = EDGE_CURVE ( 'NONE', #18977, #14601, #15269, .T. ) ;
#8509 = ORIENTED_EDGE ( 'NONE', *, *, #20655, .T. ) ;
#8510 = DIRECTION ( 'NONE',  ( 0.9387810623359078566, 0.3426822732243069436, 0.03548206049944095664 ) ) ;
#8511 = ORIENTED_EDGE ( 'NONE', *, *, #14257, .T. ) ;
#8512 =( BOUNDED_CURVE ( )  B_SPLINE_CURVE ( 2, ( #11973, #505, #18702, #5360, #3386, #8787, #5041, #13414, #20148, #76, #12076, #404, #15599 ),
 .UNSPECIFIED., .F., .F. ) 
 B_SPLINE_CURVE_WITH_KNOTS ( ( 3, 2, 2, 2, 2, 2, 3 ),
 ( 0.3455882352941176405, 0.3470588235294117530, 0.3499999999999999778, 0.3529411764705882582, 0.3558823529411764830, 0.3588235294117647078, 0.3602941176470588203 ),
 .UNSPECIFIED. ) 
 CURVE ( )  GEOMETRIC_REPRESENTATION_ITEM ( )  RATIONAL_B_SPLINE_CURVE ( ( 0.9755282581475768211, 0.9755282581475768211, 1.000000000000000000, 0.9510565162951535312, 1.000000000000000000, 0.9510565162951535312, 1.000000000000000000, 0.9510565162951535312, 1.000000000000000000, 0.9510565162951535312, 1.000000000000000000, 0.9755282581475768211, 0.9755282581475768211 ) ) 
 REPRESENTATION_ITEM ( '' )  );
#8513 = CARTESIAN_POINT ( 'NONE',  ( 43.01140435219951286, 102.5344580088725763, 39.46799094044489209 ) ) ;
#8514 = CARTESIAN_POINT ( 'NONE',  ( 40.27526882409969744, 155.9297705074273210, 30.44471234641812174 ) ) ;
#8515 = CARTESIAN_POINT ( 'NONE',  ( 39.42975644700377558, 63.67977050742732104, 36.81289934271958941 ) ) ;
#8517 = CARTESIAN_POINT ( 'NONE',  ( 26.92635752117756098, 142.9018661569831750, -16.76761354414967542 ) ) ;
#8516 = CARTESIAN_POINT ( 'NONE',  ( 47.43856463449117200, 115.4651871740940123, 35.64915139335016647 ) ) ;
#8518 = CARTESIAN_POINT ( 'NONE',  ( 41.46631938032478359, 84.11049967264874283, 29.45539723777780239 ) ) ;
#8519 = DIRECTION ( 'NONE',  ( 0.000000000000000000, 0.000000000000000000, 1.000000000000000000 ) ) ;
#8520 = CARTESIAN_POINT ( 'NONE',  ( -149.8854112254399240, -171.7362167067689995, 59.65701158161632378 ) ) ;
#8521 = LINE ( 'NONE', #6761, #9991 ) ;
#8522 = CARTESIAN_POINT ( 'NONE',  ( 45.74753988029933538, 77.06518717409399244, 30.44471234641811819 ) ) ;
#8523 = CARTESIAN_POINT ( 'NONE',  ( 39.96017580440467043, 144.7216711109867049, 30.23627618186983312 ) ) ;
#8524 = LINE ( 'NONE', #6657, #17999 ) ;
#8525 = EDGE_CURVE ( 'NONE', #488, #4466, #12273, .T. ) ;
#8526 = ORIENTED_EDGE ( 'NONE', *, *, #5294, .F. ) ;
#8527 = CARTESIAN_POINT ( 'NONE',  ( 39.42975644700377558, 69.67977050742732104, 36.81289934271958941 ) ) ;
#8528 = CARTESIAN_POINT ( 'NONE',  ( -142.0420953463935803, -183.8084106276440366, 52.72008163687743831 ) ) ;
#8529 = CARTESIAN_POINT ( 'NONE',  ( 55.35048440753327981, 87.88826800209452017, -1.070088050731120344 ) ) ;
#8530 = CARTESIAN_POINT ( 'NONE',  ( -142.0420953463935803, -174.5084106276440252, 46.59394152635518793 ) ) ;
#8531 = VERTEX_POINT ( 'NONE', #18896 ) ;
#8532 = AXIS2_PLACEMENT_3D ( 'NONE', #13473, #8629, #15238 ) ;
#8533 = CARTESIAN_POINT ( 'NONE',  ( 46.59305225739526435, 154.3151871740940067, 36.81289934271958941 ) ) ;
#8534 = AXIS2_PLACEMENT_3D ( 'NONE', #13901, #20640, #11931 ) ;
#8535 = CARTESIAN_POINT ( 'NONE',  ( 43.01140435219951996, 10.71049967264875491, 34.21067981925357060 ) ) ;
#8536 = CARTESIAN_POINT ( 'NONE',  ( 9.021810916323596885, 123.9851095102452945, 2.220310480865780534 ) ) ;
#8537 = ORIENTED_EDGE ( 'NONE', *, *, #5560, .F. ) ;
#8538 = PRODUCT_DEFINITION ( 'UNKNOWN', '', #6326, #5311 ) ;
#8539 = AXIS2_PLACEMENT_3D ( 'NONE', #11096, #13079, #17808 ) ;
#8540 = ORIENTED_EDGE ( 'NONE', *, *, #6726, .F. ) ;
#8541 = CARTESIAN_POINT ( 'NONE',  ( 39.92123440845005433, 126.2604996726487343, 29.95742577749336988 ) ) ;
#8542 = CARTESIAN_POINT ( 'NONE',  ( 44.37947211624943833, 158.2151871740939839, 30.00020018409699318 ) ) ;
#8543 = CARTESIAN_POINT ( 'NONE',  ( 38.34086628137072239, 86.07498427433979771, 8.486398261126511855 ) ) ;
#8544 = VECTOR ( 'NONE', #19491, 1000.000000000000000 ) ;
#8545 = CARTESIAN_POINT ( 'NONE',  ( 43.80332655382220253, 81.61133943119283174, 39.21067981925355639 ) ) ;
#8546 = DIRECTION ( 'NONE',  ( 0.000000000000000000, 0.000000000000000000, 1.000000000000000000 ) ) ;
#8547 = CARTESIAN_POINT ( 'NONE',  ( -148.3790856849358306, -181.5891397928654669, 59.16757674456786020 ) ) ;
#8548 = EDGE_CURVE ( 'NONE', #13406, #19098, #13505, .T. ) ;
#8549 = CARTESIAN_POINT ( 'NONE',  ( 46.10157429594899270, 101.6604996726487258, 29.95742577749336988 ) ) ;
#8550 = CARTESIAN_POINT ( 'NONE',  ( -151.4692556286852891, -196.9891397928655010, 39.65701158161630246 ) ) ;
#8551 = CARTESIAN_POINT ( 'NONE',  ( 43.01140435219951286, 77.96049967264873715, 29.21067981925356705 ) ) ;
#8552 = DIRECTION ( 'NONE',  ( 0.000000000000000000, 0.000000000000000000, -1.000000000000000000 ) ) ;
#8553 = CARTESIAN_POINT ( 'NONE',  ( 47.43856463449117200, 95.02977050742730114, 32.77220824515698183 ) ) ;
#8554 = CARTESIAN_POINT ( 'NONE',  ( 50.11350838007777497, 92.61696660072725251, -6.867350599827054758 ) ) ;
#8555 = CARTESIAN_POINT ( 'NONE',  ( -157.2955611005346270, -176.3438272943106710, 41.63779006702063867 ) ) ;
#8556 = CARTESIAN_POINT ( 'NONE',  ( 40.27526882409969744, 77.66518717409400097, 30.44471234641812174 ) ) ;
#8557 = CARTESIAN_POINT ( 'NONE',  ( 43.01140435219951996, 10.71049967264875491, 34.21067981925357060 ) ) ;
#8558 = ORIENTED_EDGE ( 'NONE', *, *, #2850, .F. ) ;
#8559 = LINE ( 'NONE', #5027, #14343 ) ;
#8560 = CARTESIAN_POINT ( 'NONE',  ( 21.90415124324598750, 92.95514585177724598, 15.07745334355238676 ) ) ;
#8561 = CARTESIAN_POINT ( 'NONE',  ( 70.72621728061167801, 115.1542034346632875, -7.148670959876664455 ) ) ;
#8562 = DIRECTION ( 'NONE',  ( 0.000000000000000000, 1.000000000000000000, 0.000000000000000000 ) ) ;
#8563 = EDGE_LOOP ( 'NONE', ( #16614, #2, #8414, #952 ) ) ;
#8564 = CARTESIAN_POINT ( 'NONE',  ( 39.42975644700377558, 147.6797705074273495, 36.81289934271958941 ) ) ;
#8565 = EDGE_CURVE ( 'NONE', #18253, #13487, #18870, .T. ) ;
#8566 = CARTESIAN_POINT ( 'NONE',  ( 45.74753988029933538, 100.4297705074273210, 37.97664729208901946 ) ) ;
#8567 = CARTESIAN_POINT ( 'NONE',  ( 48.01140435219951996, 152.2104996726487514, 34.21067981925357060 ) ) ;
#8568 = DIRECTION ( 'NONE',  ( 0.000000000000000000, 0.000000000000000000, 1.000000000000000000 ) ) ;
#8569 = CARTESIAN_POINT ( 'NONE',  ( 43.01140435219951286, 95.96049967264873715, 29.21067981925356705 ) ) ;
#8570 =( BOUNDED_CURVE ( )  B_SPLINE_CURVE ( 2, ( #12241, #10386, #17087, #555, #19083, #10708, #2001, #8732, #15450, #15551, #7185, #350, #7080 ),
 .UNSPECIFIED., .F., .F. ) 
 B_SPLINE_CURVE_WITH_KNOTS ( ( 3, 2, 2, 2, 2, 2, 3 ),
 ( 0.3455882352941176405, 0.3470588235294117530, 0.3499999999999999778, 0.3529411764705882582, 0.3558823529411764830, 0.3588235294117647078, 0.3602941176470588203 ),
 .UNSPECIFIED. ) 
 CURVE ( )  GEOMETRIC_REPRESENTATION_ITEM ( )  RATIONAL_B_SPLINE_CURVE ( ( 0.9755282581475768211, 0.9755282581475768211, 1.000000000000000000, 0.9510565162951535312, 1.000000000000000000, 0.9510565162951535312, 1.000000000000000000, 0.9510565162951535312, 1.000000000000000000, 0.9510565162951535312, 1.000000000000000000, 0.9755282581475768211, 0.9755282581475768211 ) ) 
 REPRESENTATION_ITEM ( '' )  );
#8571 = CYLINDRICAL_SURFACE ( 'NONE', #21034, 24.99999999999998934 ) ;
#8572 = FACE_OUTER_BOUND ( 'NONE', #16584, .T. ) ;
#8573 = CARTESIAN_POINT ( 'NONE',  ( -148.3790856849358306, -165.6630981290892919, 59.16757674456786020 ) ) ;
#8574 = CARTESIAN_POINT ( 'NONE',  ( 44.55648932407425633, 139.8844580088725991, 29.45539723777780239 ) ) ;
#8575 = CARTESIAN_POINT ( 'NONE',  ( 47.43856463449118621, 121.8797705074273239, 34.21067981925357060 ) ) ;
#8576 = CARTESIAN_POINT ( 'NONE',  ( 16.32863300717066579, 110.5331391746388761, 0.7949662885976053195 ) ) ;
#8577 = CARTESIAN_POINT ( 'NONE',  ( 40.27526882409969744, 114.5651871740939924, 37.97664729208901235 ) ) ;
#8578 = DIRECTION ( 'NONE',  ( 0.000000000000000000, 0.000000000000000000, 1.000000000000000000 ) ) ;
#8579 = CARTESIAN_POINT ( 'NONE',  ( 77.15557362092413030, 120.6950048976143250, -0.4420599252208967100 ) ) ;
#8580 = ADVANCED_FACE ( 'NONE', ( #20345 ), #3371, .T. ) ;
#8581 = CARTESIAN_POINT ( 'NONE',  ( 24.25535704844963547, 98.85002770340597067, 1.227849354118501601 ) ) ;
#8582 = CARTESIAN_POINT ( 'NONE',  ( 45.22504609509771001, 59.11591859955431971, 30.37668211462113277 ) ) ;
#8583 = CARTESIAN_POINT ( 'NONE',  ( 43.01140435219951286, 82.12977050742730967, 38.86567161673127657 ) ) ;
#8584 = ORIENTED_EDGE ( 'NONE', *, *, #15692, .T. ) ;
#8585 = ADVANCED_FACE ( 'NONE', ( #3803 ), #6900, .T. ) ;
#8586 = CARTESIAN_POINT ( 'NONE',  ( 41.46631938032478359, 69.38445800887258486, 38.96596240072933170 ) ) ;
#8587 = CARTESIAN_POINT ( 'NONE',  ( 38.01140435219952707, 86.78445800887257633, 34.21067981925357060 ) ) ;
#8588 = CARTESIAN_POINT ( 'NONE',  ( 48.01140435219951996, 128.2104996726487514, 34.21067981925357060 ) ) ;
#8590 = CARTESIAN_POINT ( 'NONE',  ( 76.07019559177007295, 111.3280993686123281, -14.13269547130637704 ) ) ;
#8589 = CARTESIAN_POINT ( 'NONE',  ( 47.43856463449117200, 85.76518717409398107, 32.77220824515698183 ) ) ;
#8591 = CARTESIAN_POINT ( 'NONE',  ( -161.4692556286853176, -194.4891397928654726, 49.65701158161630957 ) ) ;
#8592 = CARTESIAN_POINT ( 'NONE',  ( -145.6429501568359797, -180.8438272943106995, 57.67623309621197336 ) ) ;
#8593 = CARTESIAN_POINT ( 'NONE',  ( 38.01140435219952707, 116.6344580088725706, 32.58608133808903773 ) ) ;
#8594 = CARTESIAN_POINT ( 'NONE',  ( -148.3790856849358306, -194.4630981290893317, 40.14644641866477315 ) ) ;
#8595 =( REPRESENTATION_RELATIONSHIP ('NONE','NONE', #6933, #13805 ) REPRESENTATION_RELATIONSHIP_WITH_TRANSFORMATION ( #9983 )SHAPE_REPRESENTATION_RELATIONSHIP( ) );
#8596 = FACE_OUTER_BOUND ( 'NONE', #20913, .T. ) ;
#8597 = CARTESIAN_POINT ( 'NONE',  ( 41.64333658814960870, 147.9797705074273324, 38.42115945441014446 ) ) ;
#8598 = CARTESIAN_POINT ( 'NONE',  ( -153.0531000319306827, -183.8899795514095672, 59.65701158161631668 ) ) ;
#8599 = CARTESIAN_POINT ( 'NONE',  ( 26.66797635711824199, 149.9459070286683868, 17.30505193804556185 ) ) ;
#8600 = CARTESIAN_POINT ( 'NONE',  ( 45.74753988029934249, 143.0651871740939782, 30.44471234641812174 ) ) ;
#8601 = CARTESIAN_POINT ( 'NONE',  ( -156.1828648351502125, -155.3945647575688156, 41.49286807254280518 ) ) ;
#8602 = CARTESIAN_POINT ( 'NONE',  ( -160.8964159109769696, -173.3084106276440366, 46.59394152635518083 ) ) ;
#8603 = CARTESIAN_POINT ( 'NONE',  ( 38.58424406990786082, 63.11518717409400381, 34.21067981925357060 ) ) ;
#8604 = CARTESIAN_POINT ( 'NONE',  ( -159.0959885057557983, -164.4584106276440423, 44.11586579668791330 ) ) ;
#8605 = CIRCLE ( 'NONE', #20917, 4.999999999999997335 ) ;
#8606 = CARTESIAN_POINT ( 'NONE',  ( 70.95506224315714405, 115.5552942049593668, 4.842541188697900623 ) ) ;
#8607 = CARTESIAN_POINT ( 'NONE',  ( -151.4692556286852891, -196.9891397928655010, 59.65701158161632378 ) ) ;
#8608 = CARTESIAN_POINT ( 'NONE',  ( 41.64333658814960870, 125.5151871740939953, 30.00020018409699318 ) ) ;
#8609 = SHAPE_REPRESENTATION ( 'bolt', ( #12657 ), #7417 ) ;
#8610 = VERTEX_POINT ( 'NONE', #5239 ) ;
#8611 = VERTEX_POINT ( 'NONE', #8450 ) ;
#8612 = ADVANCED_FACE ( 'NONE', ( #20238 ), #15156, .T. ) ;
#8613 = CARTESIAN_POINT ( 'NONE',  ( 38.01140435219952707, 113.6344580088725706, 32.58608133808903773 ) ) ;
#8614 = ORIENTED_EDGE ( 'NONE', *, *, #12987, .T. ) ;
#8615 = CARTESIAN_POINT ( 'NONE',  ( 39.92123440845004723, 102.2344580088725650, 38.46393386101376421 ) ) ;
#8616 = CARTESIAN_POINT ( 'NONE',  ( 38.58424406990785371, 156.2297705074273040, 32.77220824515697473 ) ) ;
#8617 = CARTESIAN_POINT ( 'NONE',  ( 39.92123440845004723, 156.2604996726486775, 29.95742577749337343 ) ) ;
#8619 = CARTESIAN_POINT ( 'NONE',  ( 29.48178659935447854, 144.5857871963822845, 17.33364154221121467 ) ) ;
#8618 = CARTESIAN_POINT ( 'NONE',  ( 45.74753988029933538, 119.0651871740939782, 30.44471234641811819 ) ) ;
#8620 = CIRCLE ( 'NONE', #18104, 13.99821153497579651 ) ;
#8621 = CARTESIAN_POINT ( 'NONE',  ( 44.55648932407425633, 80.81049967264873146, 29.45539723777780239 ) ) ;
#8622 = CARTESIAN_POINT ( 'NONE',  ( 38.96631938032478359, 75.08445800887257349, 37.14960608071593384 ) ) ;
#8623 = DIRECTION ( 'NONE',  ( 0.000000000000000000, 1.000000000000000000, 0.000000000000000000 ) ) ;
#8624 = FACE_OUTER_BOUND ( 'NONE', #8885, .T. ) ;
#8625 = AXIS2_PLACEMENT_3D ( 'NONE', #12218, #2196, #7276 ) ;
#8626 = CARTESIAN_POINT ( 'NONE',  ( 38.58424406990786082, 75.11518717409400381, 34.21067981925357060 ) ) ;
#8627 = CARTESIAN_POINT ( 'NONE',  ( 38.17209587424806472, 144.4343147008670485, 32.91136586774996431 ) ) ;
#8628 = CARTESIAN_POINT ( 'NONE',  ( 38.96631938032478359, 122.4844580088725934, 31.27175355779120025 ) ) ;
#8629 = DIRECTION ( 'NONE',  ( 0.000000000000000000, 0.000000000000000000, 1.000000000000000000 ) ) ;
#8630 = EDGE_LOOP ( 'NONE', ( #19998, #3812, #10096, #19794 ) ) ;
#8631 = CARTESIAN_POINT ( 'NONE',  ( -145.6429501568359797, -184.1084106276440480, 57.67623309621198047 ) ) ;
#8632 = CARTESIAN_POINT ( 'NONE',  ( 9.231363607564425422, 125.4582397780895633, 16.26765482522027639 ) ) ;
#8633 = CARTESIAN_POINT ( 'NONE',  ( -142.0420953463935803, -180.5084106276440536, 46.59394152635518793 ) ) ;
#8634 = ORIENTED_EDGE ( 'NONE', *, *, #19108, .T. ) ;
#8635 = CARTESIAN_POINT ( 'NONE',  ( 44.37947211624943833, 158.2151871740939839, 30.00020018409699318 ) ) ;
#8636 = FACE_OUTER_BOUND ( 'NONE', #5423, .T. ) ;
#8637 = CARTESIAN_POINT ( 'NONE',  ( 46.59305225739526435, 118.5797705074273267, 36.81289934271958941 ) ) ;
#8638 = CARTESIAN_POINT ( 'NONE',  ( 42.92180000979148957, 85.67454126555050209, 7.339147150375312734 ) ) ;
#8639 = EDGE_LOOP ( 'NONE', ( #8419, #6145 ) ) ;
#8640 = CARTESIAN_POINT ( 'NONE',  ( 71.19430100617981338, 118.9508470517051535, -8.295922056425867552 ) ) ;
#8641 = ORIENTED_EDGE ( 'NONE', *, *, #15855, .T. ) ;
#8642 = CARTESIAN_POINT ( 'NONE',  ( 47.43856463449117200, 109.7297705074273040, 35.64915139335016647 ) ) ;
#8643 = CARTESIAN_POINT ( 'NONE',  ( 41.46631938032478359, 158.1844580088726104, 29.45539723777780239 ) ) ;
#8644 = PLANE ( 'NONE',  #14648 ) ;
#8645 = AXIS2_PLACEMENT_3D ( 'NONE', #14055, #4343, #15812 ) ;
#8646 = CARTESIAN_POINT ( 'NONE',  ( 39.42975644700377558, 143.8151871740940067, 31.60846029578754468 ) ) ;
#8647 = CARTESIAN_POINT ( 'NONE',  ( 30.24639091383375700, 151.6717570033048048, 3.410403464249057492 ) ) ;
#8648 = PLANE ( 'NONE',  #15227 ) ;
#8649 = DIRECTION ( 'NONE',  ( 0.000000000000000000, 0.000000000000000000, 1.000000000000000000 ) ) ;
#8650 = CARTESIAN_POINT ( 'NONE',  ( -143.3790856849358306, -168.6891397928654897, 43.77915905869157598 ) ) ;
#8651 = CARTESIAN_POINT ( 'NONE',  ( -153.0531000319306827, -180.8899795514095956, 59.65701158161632378 ) ) ;
#8652 = UNCERTAINTY_MEASURE_WITH_UNIT (LENGTH_MEASURE( 1.000000000000000082E-05 ), #20926, 'distance_accuracy_value', 'NONE');
#8653 = CARTESIAN_POINT ( 'NONE',  ( 79.42064422693164261, 282.0082918409407284, 4.000000000000003553 ) ) ;
#8654 = PLANE ( 'NONE',  #8020 ) ;
#8655 = EDGE_CURVE ( 'NONE', #10182, #12281, #10941, .T. ) ;
#8656 = CARTESIAN_POINT ( 'NONE',  ( 45.74753988029933538, 97.42977050742730682, 37.97664729208901946 ) ) ;
#8657 = CARTESIAN_POINT ( 'NONE',  ( 59.92122946415073415, 142.4742691614619332, -9.367183195626855863 ) ) ;
#8658 = CARTESIAN_POINT ( 'NONE',  ( -154.3824083646099439, -170.4938272943107336, 40.69124936498395328 ) ) ;
#8659 = CARTESIAN_POINT ( 'NONE',  ( 44.37947211624943833, 80.21518717409399812, 30.00020018409699318 ) ) ;
#8660 = DIRECTION ( 'NONE',  ( 1.000000000000000000, 0.000000000000000000, 0.000000000000000000 ) ) ;
#8661 = CARTESIAN_POINT ( 'NONE',  ( -154.5594255724347761, -159.0891397928654953, 40.14644641866476604 ) ) ;
#8662 = AXIS2_PLACEMENT_3D ( 'NONE', #18116, #9763, #16460 ) ;
#8663 = VERTEX_POINT ( 'NONE', #1824 ) ;
#8664 = FACE_OUTER_BOUND ( 'NONE', #6770, .T. ) ;
#8665 = CARTESIAN_POINT ( 'NONE',  ( 68.96269327682742301, 142.1111764150114993, -15.20387477620461425 ) ) ;
#8666 = ORIENTED_EDGE ( 'NONE', *, *, #11528, .T. ) ;
#8667 = LINE ( 'NONE', #2048, #4434 ) ;
#8668 = ORIENTED_EDGE ( 'NONE', *, *, #17575, .F. ) ;
#8669 = CARTESIAN_POINT ( 'NONE',  ( 47.43856463449117200, 137.0297705074272869, 32.77220824515698183 ) ) ;
#8670 = AXIS2_PLACEMENT_3D ( 'NONE', #9901, #8249, #21697 ) ;
#8671 = CARTESIAN_POINT ( 'NONE',  ( -151.4692556286852891, -180.8130981290893260, 59.65701158161631668 ) ) ;
#8672 = AXIS2_PLACEMENT_3D ( 'NONE', #3078, #9814, #20070 ) ;
#8673 = CARTESIAN_POINT ( 'NONE',  ( 108.9927164799167372, 227.3511983043831037, -5.999999999999976019 ) ) ;
#8674 = CARTESIAN_POINT ( 'NONE',  ( 43.01140435219951286, 102.5344580088725763, 39.21067981925356349 ) ) ;
#8675 = DIRECTION ( 'NONE',  ( -1.000000000000000000, 0.000000000000000000, 0.000000000000000000 ) ) ;
#8676 = CARTESIAN_POINT ( 'NONE',  ( 38.01140435219952707, 108.5604996726487457, 32.58608133808903773 ) ) ;
#8677 = CARTESIAN_POINT ( 'NONE',  ( -161.4692556286853176, -172.5630981290893260, 49.65701158161630957 ) ) ;
#8678 = DIRECTION ( 'NONE',  ( 0.9183650514339934956, 0.000000000000000000, -0.3957342950827467121 ) ) ;
#8679 = CARTESIAN_POINT ( 'NONE',  ( 44.55648932407425633, 138.6844580088725820, 38.96596240072933170 ) ) ;
#8680 = CARTESIAN_POINT ( 'NONE',  ( 46.59305225739526435, 122.1797705074273210, 31.60846029578754468 ) ) ;
#8681 = CARTESIAN_POINT ( 'NONE',  ( 35.43645570112151688, 92.65990651318493576, -0.2767073223962682738 ) ) ;
#8682 = CARTESIAN_POINT ( 'NONE',  ( 46.10157429594899270, 99.83445800887257349, 38.46393386101375711 ) ) ;
#8683 = CARTESIAN_POINT ( 'NONE',  ( 44.37947211624943833, 110.2151871740940123, 30.00020018409699318 ) ) ;
#8684 = PLANE ( 'NONE',  #7335 ) ;
#8685 = CARTESIAN_POINT ( 'NONE',  ( 23.67598417054553295, 91.65793073385727041, -5.994147020910363999 ) ) ;
#8686 = CARTESIAN_POINT ( 'NONE',  ( 57.86150831142030171, 95.93494642397840266, -0.2007220744356660869 ) ) ;
#8687 = PRODUCT ( 'MAS-327', 'MAS-327', '', ( #12623 ) ) ;
#8688 = VECTOR ( 'NONE', #2410, 1000.000000000000000 ) ;
#8689 = CARTESIAN_POINT ( 'NONE',  ( -148.3790856849358306, -185.4630981290893033, 40.14644641866477315 ) ) ;
#8690 = ADVANCED_FACE ( 'NONE', ( #7115 ), #17018, .T. ) ;
#8691 = CARTESIAN_POINT ( 'NONE',  ( 41.64333658814960870, 86.77977050742731535, 30.00020018409699318 ) ) ;
#8692 = VECTOR ( 'NONE', #5226, 1000.000000000000000 ) ;
#8693 = EDGE_CURVE ( 'NONE', #16672, #6394, #1930, .T. ) ;
#8694 = ORIENTED_EDGE ( 'NONE', *, *, #6520, .F. ) ;
#8695 = CARTESIAN_POINT ( 'NONE',  ( 48.01140435219951996, 110.3604996726487428, 32.58608133808903773 ) ) ;
#8696 =( BOUNDED_CURVE ( )  B_SPLINE_CURVE ( 2, ( #5144, #403, #17033, #2055, #12075, #15501, #11863, #13620, #7133, #17246, #8897, #10655, #13837 ),
 .UNSPECIFIED., .F., .F. ) 
 B_SPLINE_CURVE_WITH_KNOTS ( ( 3, 2, 2, 2, 2, 2, 3 ),
 ( 0.05147058823529411520, 0.05294117647058823456, 0.05588235294117647328, 0.05882352941176470507, 0.06176470588235294379, 0.06470588235294118251, 0.06617647058823528106 ),
 .UNSPECIFIED. ) 
 CURVE ( )  GEOMETRIC_REPRESENTATION_ITEM ( )  RATIONAL_B_SPLINE_CURVE ( ( 0.9755282581475767101, 0.9755282581475765991, 1.000000000000000000, 0.9510565162951535312, 1.000000000000000000, 0.9510565162951535312, 1.000000000000000000, 0.9510565162951535312, 1.000000000000000000, 0.9510565162951535312, 1.000000000000000000, 0.9755282581475769321, 0.9755282581475765991 ) ) 
 REPRESENTATION_ITEM ( '' )  );
#8697 = CARTESIAN_POINT ( 'NONE',  ( 46.10157429594899270, 72.83445800887257349, 38.46393386101376421 ) ) ;
#8698 = CARTESIAN_POINT ( 'NONE',  ( 41.46631938032478359, 126.1104996726487570, 29.45539723777780239 ) ) ;
#8700 = CARTESIAN_POINT ( 'NONE',  ( 71.19781441516849441, 139.1947734567256703, -15.08494495145127878 ) ) ;
#8699 = CARTESIAN_POINT ( 'NONE',  ( 41.64333658814960870, 84.71518717409399812, 38.42115945441014446 ) ) ;
#8701 = CIRCLE ( 'NONE', #5188, 5.000000000000004441 ) ;
#8702 = CARTESIAN_POINT ( 'NONE',  ( -154.3824083646099439, -155.7584106276440536, 40.69124936498395328 ) ) ;
#8703 = CARTESIAN_POINT ( 'NONE',  ( -142.0420953463935803, -183.2438272943107336, 46.59394152635518083 ) ) ;
#8704 = CARTESIAN_POINT ( 'NONE',  ( -141.4692556286852891, -178.1391397928654499, 52.90620854394536821 ) ) ;
#8705 = FACE_OUTER_BOUND ( 'NONE', #3260, .T. ) ;
#8706 = DIRECTION ( 'NONE',  ( 0.000000000000000000, 0.000000000000000000, 1.000000000000000000 ) ) ;
#8707 = CARTESIAN_POINT ( 'NONE',  ( 47.05648932407426344, 67.91049967264873999, 37.14960608071593384 ) ) ;
#8708 = CARTESIAN_POINT ( 'NONE',  ( 46.10157429594899270, 142.7604996726487343, 38.46393386101375711 ) ) ;
#8709 = CARTESIAN_POINT ( 'NONE',  ( 38.58424406990784661, 147.5297705074273154, 35.64915139335016647 ) ) ;
#8710 = CARTESIAN_POINT ( 'NONE',  ( 46.59305225739526435, 106.5797705074273125, 36.81289934271958941 ) ) ;
#8711 = CARTESIAN_POINT ( 'NONE',  ( 11.08170843061617816, 132.1625483722078513, 16.49545033792581350 ) ) ;
#8712 = CARTESIAN_POINT ( 'NONE',  ( 44.37947211624943833, 131.2151871740940123, 30.00020018409699318 ) ) ;
#8713 = CYLINDRICAL_SURFACE ( 'NONE', #13876, 4.999999999999997335 ) ;
#8714 = CARTESIAN_POINT ( 'NONE',  ( -142.0420953463935803, -177.8084106276440366, 52.72008163687743831 ) ) ;
#8715 = CARTESIAN_POINT ( 'NONE',  ( 41.64333658814960870, 59.51518717409400239, 30.00020018409699318 ) ) ;
#8716 = CARTESIAN_POINT ( 'NONE',  ( 20.64193819951031017, 102.6032774297415102, 0.4378519886423143381 ) ) ;
#8717 = CARTESIAN_POINT ( 'NONE',  ( 42.21948215057684450, 135.4575765865523067, 39.21067981925355639 ) ) ;
#8718 = CARTESIAN_POINT ( 'NONE',  ( 40.27526882409969033, 114.5651871740939782, 37.97664729208901946 ) ) ;
#8719 = VECTOR ( 'NONE', #19026, 1000.000000000000114 ) ;
#8720 = ORIENTED_EDGE ( 'NONE', *, *, #12097, .T. ) ;
#8721 = PLANE ( 'NONE',  #13104 ) ;
#8722 = ORIENTED_EDGE ( 'NONE', *, *, #14123, .F. ) ;
#8723 = CARTESIAN_POINT ( 'NONE',  ( 48.01140435219951996, 103.2844580088725763, 34.21067981925357060 ) ) ;
#8724 = CARTESIAN_POINT ( 'NONE',  ( 38.58424406990785371, 153.2297705074273324, 32.77220824515697473 ) ) ;
#8725 = CARTESIAN_POINT ( 'NONE',  ( 45.74753988029933538, 62.32977050742730540, 30.44471234641811819 ) ) ;
#8727 = CARTESIAN_POINT ( 'NONE',  ( 60.58642193167724344, 97.95666160567475345, -13.33918631239395225 ) ) ;
#8726 = CARTESIAN_POINT ( 'NONE',  ( 38.58424406990784661, 116.9651871740939839, 32.77220824515698183 ) ) ;
#8728 = AXIS2_PLACEMENT_3D ( 'NONE', #16220, #6192, #4321 ) ;
#8729 = CARTESIAN_POINT ( 'NONE',  ( 38.01140435219951996, 72.56049967264874567, 32.58608133808903773 ) ) ;
#8731 = DIRECTION ( 'NONE',  ( 0.000000000000000000, 0.000000000000000000, 1.000000000000000000 ) ) ;
#8730 = DIRECTION ( 'NONE',  ( -0.000000000000000000, -1.000000000000000000, -0.000000000000000000 ) ) ;
#8732 = CARTESIAN_POINT ( 'NONE',  ( 38.01140435219952707, 123.5604996726487173, 32.58608133808903773 ) ) ;
#8733 = CARTESIAN_POINT ( 'NONE',  ( 46.77777258146056738, 95.19132504939746298, 37.51526355657936307 ) ) ;
#8734 = CARTESIAN_POINT ( 'NONE',  ( 40.27526882409969033, 81.56518717409399244, 37.97664729208901946 ) ) ;
#8735 = CARTESIAN_POINT ( 'NONE',  ( 38.26853956736072604, 144.4533880425008192, 35.82660397859488199 ) ) ;
#8736 = AXIS2_PLACEMENT_3D ( 'NONE', #19111, #7538, #5653 ) ;
#8737 = CARTESIAN_POINT ( 'NONE',  ( -145.6429501568359797, -180.8438272943106995, 57.67623309621198047 ) ) ;
#8738 = CARTESIAN_POINT ( 'NONE',  ( 57.67197451322208934, 240.2871645992278218, 0.000000000000000000 ) ) ;
#8739 = ADVANCED_FACE ( 'NONE', ( #1029 ), #4226, .F. ) ;
#8740 = EDGE_LOOP ( 'NONE', ( #1274, #14179, #4465, #17531 ) ) ;
#8741 = CARTESIAN_POINT ( 'NONE',  ( -157.2955611005346270, -185.6084106276440195, 41.63779006702063867 ) ) ;
#8742 = CARTESIAN_POINT ( 'NONE',  ( 38.54497605562327323, 85.96704844161884296, 14.48200433579215662 ) ) ;
#8743 = CARTESIAN_POINT ( 'NONE',  ( -142.0420953463936087, -180.6584106276440309, 49.65701158161630957 ) ) ;
#8744 = ORIENTED_EDGE ( 'NONE', *, *, #12977, .T. ) ;
#8745 = CARTESIAN_POINT ( 'NONE',  ( 47.43856463449118621, 139.6151871740939896, 34.21067981925357060 ) ) ;
#8746 = CARTESIAN_POINT ( 'NONE',  ( 0.000000000000000000, -126.9891397928655010, 0.000000000000000000 ) ) ;
#8747 = CARTESIAN_POINT ( 'NONE',  ( 44.37947211624943833, 101.4797705074273182, 30.00020018409699318 ) ) ;
#8748 = CARTESIAN_POINT ( 'NONE',  ( 10.16827731527805767, 110.2528774685086574, 8.767718578943870966 ) ) ;
#8749 = ORIENTED_EDGE ( 'NONE', *, *, #15855, .F. ) ;
#8750 = CARTESIAN_POINT ( 'NONE',  ( 17.24633477965345918, 131.3686459745448758, -4.367463884209165315 ) ) ;
#8751 = ORIENTED_EDGE ( 'NONE', *, *, #18616, .T. ) ;
#8752 = CARTESIAN_POINT ( 'NONE',  ( 38.58424406990784661, 111.5297705074273154, 35.64915139335016647 ) ) ;
#8753 = CARTESIAN_POINT ( 'NONE',  ( 38.96631938032478359, 131.4844580088725934, 31.27175355779120025 ) ) ;
#8754 = CARTESIAN_POINT ( 'NONE',  ( 38.01140435219952707, 126.5604996726487315, 32.58608133808903773 ) ) ;
#8755 = CARTESIAN_POINT ( 'NONE',  ( 41.64333658814960870, 141.7151871740940123, 38.42115945441014446 ) ) ;
#8756 = CARTESIAN_POINT ( 'NONE',  ( 41.46631938032478359, 100.3104996726487457, 38.96596240072933170 ) ) ;
#8757 = CARTESIAN_POINT ( 'NONE',  ( 54.54805624998882507, 152.1374805055981199, -2.779977617235711129 ) ) ;
#8758 = CARTESIAN_POINT ( 'NONE',  ( -141.4692556286852891, -180.0630981290892976, 49.65701158161630957 ) ) ;
#8759 = CARTESIAN_POINT ( 'NONE',  ( -141.4692556286852891, -169.1391397928654214, 52.90620854394536821 ) ) ;
#8760 = CARTESIAN_POINT ( 'NONE',  ( 43.01140435219951286, 100.4604996726487371, 39.21067981925356349 ) ) ;
#8761 = CARTESIAN_POINT ( 'NONE',  ( -151.4692556286852891, -195.2391397928655010, 39.65701158161629536 ) ) ;
#8762 = EDGE_CURVE ( 'NONE', #13207, #13022, #20770, .T. ) ;
#8763 = DIRECTION ( 'NONE',  ( 1.000000000000000000, 0.000000000000000000, 0.000000000000000000 ) ) ;
#8764 = CARTESIAN_POINT ( 'NONE',  ( -176.9699209214867608, 160.7104996726487514, -35.00000000000000000 ) ) ;
#8765 = CARTESIAN_POINT ( 'NONE',  ( 40.27526882409969033, 80.92977050742729261, 30.44471234641811819 ) ) ;
#8766 = CARTESIAN_POINT ( 'NONE',  ( 62.66823040046688931, 140.1266048904901993, -2.224326160187301227 ) ) ;
#8767 = CARTESIAN_POINT ( 'NONE',  ( -160.8964159109769696, -178.7438272943107052, 52.72008163687743121 ) ) ;
#8768 = CARTESIAN_POINT ( 'NONE',  ( 38.58424406990785371, 74.96518717409401233, 32.77220824515697473 ) ) ;
#8769 = CARTESIAN_POINT ( 'NONE',  ( 43.01140435219951286, 119.0344580088725621, 29.21067981925356705 ) ) ;
#8770 = CARTESIAN_POINT ( 'NONE',  ( -149.8854112254399524, -195.3160212151857422, 39.65701158161630246 ) ) ;
#8771 = ORIENTED_EDGE ( 'NONE', *, *, #2754, .F. ) ;
#8772 = CARTESIAN_POINT ( 'NONE',  ( 42.21948215057684450, 137.1113394311928175, 29.21067981925356705 ) ) ;
#8773 = CYLINDRICAL_SURFACE ( 'NONE', #1834, 21.90454335994854063 ) ;
#8774 = CARTESIAN_POINT ( 'NONE',  ( 46.59305225739526435, 136.5797705074272983, 36.81289934271958941 ) ) ;
#8775 = CARTESIAN_POINT ( 'NONE',  ( 61.44294336830710535, 141.1433446673695471, 5.708471897238777792 ) ) ;
#8776 = ORIENTED_EDGE ( 'NONE', *, *, #8037, .F. ) ;
#8777 = DIRECTION ( 'NONE',  ( -0.000000000000000000, -0.000000000000000000, 1.000000000000000000 ) ) ;
#8778 = VERTEX_POINT ( 'NONE', #16123 ) ;
#8779 = CARTESIAN_POINT ( 'NONE',  ( 43.01140435219951286, 140.6297705074273097, 29.55568802177586463 ) ) ;
#8780 = CARTESIAN_POINT ( 'NONE',  ( 39.42975644700377558, 93.07977050742731251, 31.60846029578754468 ) ) ;
#8781 = CARTESIAN_POINT ( 'NONE',  ( -148.3790856849358306, -181.5891397928654669, 59.16757674456786020 ) ) ;
#8782 = B_SPLINE_CURVE_WITH_KNOTS ( 'NONE', 3,
 ( #12513, #19452, #2583, #12402, #17785, #17464, #7242, #19134 ),
 .UNSPECIFIED., .F., .F.,
 ( 4, 2, 2, 4 ),
 ( 3.469446951953614189E-18, 0.001432241572422971983, 0.002148362358634445940, 0.002864483144845920114 ),
 .UNSPECIFIED. ) ;
#8783 = AXIS2_PLACEMENT_3D ( 'NONE', #4949, #18395, #11658 ) ;
#8784 = CARTESIAN_POINT ( 'NONE',  ( 41.64333658814960870, 60.71518717409399102, 38.42115945441014446 ) ) ;
#8785 = CARTESIAN_POINT ( 'NONE',  ( 38.01140435219952707, 159.7104996726487514, 34.21067981925357060 ) ) ;
#8786 = CARTESIAN_POINT ( 'NONE',  ( 38.58424406990786082, 96.11518717409400381, 34.21067981925357060 ) ) ;
#8787 = CARTESIAN_POINT ( 'NONE',  ( 38.01140435219952707, 122.9344580088725962, 35.83527830041809636 ) ) ;
#8788 = CARTESIAN_POINT ( 'NONE',  ( -161.4692556286852607, -172.4130981290892635, 52.90620854394536821 ) ) ;
#8789 = DIRECTION ( 'NONE',  ( 1.000000000000000000, 0.000000000000000000, 0.000000000000000000 ) ) ;
#8790 = CARTESIAN_POINT ( 'NONE',  ( 44.55648932407425633, 109.8844580088725849, 29.45539723777780239 ) ) ;
#8791 = CARTESIAN_POINT ( 'NONE',  ( 47.05648932407426344, 141.9844580088725650, 37.14960608071593384 ) ) ;
#8792 = CARTESIAN_POINT ( 'NONE',  ( 39.42975644700377558, 111.0797705074273125, 31.60846029578754468 ) ) ;
#8793 = CARTESIAN_POINT ( 'NONE',  ( 28.99223550982291897, 144.4690685518502846, 2.342703524990218611 ) ) ;
#8794 = CARTESIAN_POINT ( 'NONE',  ( 136.0032066456581390, 182.5367998656340944, 34.00000000000001421 ) ) ;
#8795 = CARTESIAN_POINT ( 'NONE',  ( 44.37947211624943833, 103.0151871740939953, 38.42115945441014446 ) ) ;
#8796 = LINE ( 'NONE', #1849, #6257 ) ;
#8797 = ADVANCED_FACE ( 'NONE', ( #2248 ), #10742, .F. ) ;
#8798 = CARTESIAN_POINT ( 'NONE',  ( 33.56091001181424360, 87.00402361476987778, -6.351118090676544981 ) ) ;
#8799 = CARTESIAN_POINT ( 'NONE',  ( 26.10333545525518062, 97.33820528946348816, 8.132564544556878161 ) ) ;
#8800 = CARTESIAN_POINT ( 'NONE',  ( -149.8854112254399240, -169.6622583705451746, 59.65701158161632378 ) ) ;
#8801 = CARTESIAN_POINT ( 'NONE',  ( 46.59305225739526435, 89.17977050742732104, 31.60846029578754468 ) ) ;
#8802 = ORIENTED_EDGE ( 'NONE', *, *, #14390, .T. ) ;
#8803 = PRODUCT_DEFINITION ( 'UNKNOWN', '', #1410, #3553 ) ;
#8804 = CARTESIAN_POINT ( 'NONE',  ( 38.01140435219951996, 77.93445800887256780, 35.83527830041810347 ) ) ;
#8805 = LINE ( 'NONE', #2177, #5601 ) ;
#8807 = ADVANCED_FACE ( 'NONE', ( #595 ), #21206, .T. ) ;
#8806 = CARTESIAN_POINT ( 'NONE',  ( 46.10157429594899270, 133.7604996726487059, 38.46393386101376421 ) ) ;
#8809 = CARTESIAN_POINT ( 'NONE',  ( 9.046145050308979307, 123.4917717844193277, -10.79923121120670437 ) ) ;
#8808 = CARTESIAN_POINT ( 'NONE',  ( 38.58424406990786082, 84.11518717409400381, 34.21067981925357060 ) ) ;
#8810 = CARTESIAN_POINT ( 'NONE',  ( -145.6429501568359797, -156.2084106276440423, 41.63779006702063867 ) ) ;
#8811 = CARTESIAN_POINT ( 'NONE',  ( -159.0959885057557983, -178.5938272943107279, 55.19815736654470584 ) ) ;
#8812 = DIRECTION ( 'NONE',  ( -0.9999746145782334450, 0.007125320983193089534, 0.000000000000000000 ) ) ;
#8813 = CARTESIAN_POINT ( 'NONE',  ( 46.10157429594899270, 127.7344580088725934, 29.95742577749336988 ) ) ;
#8814 = AXIS2_PLACEMENT_3D ( 'NONE', #15624, #9222, #21011 ) ;
#8815 = CARTESIAN_POINT ( 'NONE',  ( 0.000000000000000000, -136.9891397928655010, 30.00000000000000000 ) ) ;
#8816 = DIRECTION ( 'NONE',  ( 0.000000000000000000, 1.000000000000000000, 0.000000000000000000 ) ) ;
#8817 = CARTESIAN_POINT ( 'NONE',  ( 44.37947211624943833, 154.2797705074273438, 38.42115945441014446 ) ) ;
#8818 = CARTESIAN_POINT ( 'NONE',  ( 44.37947211624943833, 104.4797705074273182, 30.00020018409699318 ) ) ;
#8819 = EDGE_CURVE ( 'NONE', #5105, #12631, #2568, .T. ) ;
#8820 = CARTESIAN_POINT ( 'NONE',  ( 12.61881386508366809, 104.1535352963828984, 15.55354899318430739 ) ) ;
#8821 = CARTESIAN_POINT ( 'NONE',  ( 47.43856463449117911, 136.7651871740939953, 32.77220824515697473 ) ) ;
#8822 = CARTESIAN_POINT ( 'NONE',  ( 134.6380592378699532, 268.5785371414991687, -3.999999999999996447 ) ) ;
#8823 = CARTESIAN_POINT ( 'NONE',  ( -160.8964159109769696, -170.3084106276440082, 46.59394152635518083 ) ) ;
#8824 = CARTESIAN_POINT ( 'NONE',  ( 43.01140435219951286, 152.9604996726487798, 29.21067981925356705 ) ) ;
#8825 = CARTESIAN_POINT ( 'NONE',  ( 60.05828665636081354, 97.34093765924853869, 12.69960079420514809 ) ) ;
#8826 = ADVANCED_FACE ( 'NONE', ( #14463 ), #10855, .T. ) ;
#8827 =( LENGTH_UNIT ( ) NAMED_UNIT ( * ) SI_UNIT ( .MILLI., .METRE. ) );
#8828 = CARTESIAN_POINT ( 'NONE',  ( 39.42975644700377558, 113.8151871740940067, 31.60846029578754468 ) ) ;
#8829 =( BOUNDED_CURVE ( )  B_SPLINE_CURVE ( 2, ( #2084, #14081, #19586, #15948, #7707, #20818, #19374, #7487, #19479, #2508, #21143, #7380, #12433 ),
 .UNSPECIFIED., .F., .T. ) 
 B_SPLINE_CURVE_WITH_KNOTS ( ( 3, 2, 2, 2, 2, 2, 3 ),
 ( 0.7678571428571427937, 0.7714285714285714635, 0.7785714285714285809, 0.7857142857142856984, 0.7928571428571428159, 0.8000000000000000444, 0.8035714285714286031 ),
 .UNSPECIFIED. ) 
 CURVE ( )  GEOMETRIC_REPRESENTATION_ITEM ( )  RATIONAL_B_SPLINE_CURVE ( ( 0.9755282581475768211, 0.9755282581475763770, 1.000000000000000000, 0.9510565162951535312, 1.000000000000000000, 0.9510565162951535312, 1.000000000000000000, 0.9510565162951535312, 1.000000000000000000, 0.9510565162951535312, 1.000000000000000000, 0.9755282581475768211, 0.9755282581475768211 ) ) 
 REPRESENTATION_ITEM ( '' )  );
#8830 = EDGE_LOOP ( 'NONE', ( #5910, #16306 ) ) ;
#8831 = CLOSED_SHELL ( 'NONE', ( #8019, #19017, #9106, #19775, #9479, #15959, #19519, #11762, #10378, #677, #12731, #19566, #4874, #5823, #2774, #17783, #20611, #566, #14868, #19178, #16046, #21081, #11091, #21271, #2377, #4283, #18322, #7590, #3833, #7474, #9079, #20024, #4925, #2328, #16885, #4911, #17278, #7306, #17390, #18021, #2958, #18063, #14212, #21229, #1538, #7478, #3903, #14717, #516, #42 ) ) ;
#8832 = CARTESIAN_POINT ( 'NONE',  ( -153.0531000319306827, -159.8899795514095672, 59.65701158161631668 ) ) ;
#8833 = ORIENTED_EDGE ( 'NONE', *, *, #2664, .F. ) ;
#8834 = CARTESIAN_POINT ( 'NONE',  ( 38.01140435219951996, 101.9344580088725536, 35.83527830041810347 ) ) ;
#8835 = CARTESIAN_POINT ( 'NONE',  ( 47.43856463449117911, 151.7297705074273324, 35.64915139335015937 ) ) ;
#8836 = ADVANCED_FACE ( 'NONE', ( #16005 ), #14021, .T. ) ;
#8837 = CARTESIAN_POINT ( 'NONE',  ( 38.96631938032478359, 156.4104996726487400, 31.27175355779120025 ) ) ;
#8839 = CARTESIAN_POINT ( 'NONE',  ( 25.64412274706724304, 97.69032544021251852, 15.15625305551708202 ) ) ;
#8838 = CARTESIAN_POINT ( 'NONE',  ( 47.43856463449118621, 118.6151871740940038, 34.21067981925357060 ) ) ;
#8840 = CARTESIAN_POINT ( 'NONE',  ( 39.92123440845004723, 69.26049967264874851, 29.95742577749337343 ) ) ;
#8842 = CARTESIAN_POINT ( 'NONE',  ( 39.92123440845005433, 74.33445800887255928, 29.95742577749336988 ) ) ;
#8841 = CARTESIAN_POINT ( 'NONE',  ( 45.51311879618403822, 144.7820145757526404, 29.87844397536261098 ) ) ;
#8843 = EDGE_CURVE ( 'NONE', #16314, #1116, #8409, .T. ) ;
#8844 = CARTESIAN_POINT ( 'NONE',  ( -161.4692556286853176, -172.5630981290893260, 49.65701158161630957 ) ) ;
#8845 = CARTESIAN_POINT ( 'NONE',  ( 116.4417310231185780, -136.9891397928655010, 0.3429884183836981459 ) ) ;
#8846 = CARTESIAN_POINT ( 'NONE',  ( 39.42975644700377558, 78.41518717409400097, 36.81289934271958941 ) ) ;
#8847 = CARTESIAN_POINT ( 'NONE',  ( 43.80332655382220253, 104.8836182503284675, 29.21067981925356705 ) ) ;
#8848 = CARTESIAN_POINT ( 'NONE',  ( -151.4692556286852891, -176.6438272943107393, 39.74470866294723947 ) ) ;
#8849 = CARTESIAN_POINT ( 'NONE',  ( -142.0420953463935803, -195.5084106276440536, 46.59394152635518083 ) ) ;
#8850 = VERTEX_POINT ( 'NONE', #1346 ) ;
#8851 = CARTESIAN_POINT ( 'NONE',  ( -145.6429501568359797, -178.1084106276440480, 57.67623309621198047 ) ) ;
#8852 = CARTESIAN_POINT ( 'NONE',  ( 42.88582110127141789, 154.2205544383733695, -4.165101255777401867 ) ) ;
#8853 = ORIENTED_EDGE ( 'NONE', *, *, #11847, .T. ) ;
#8854 = CARTESIAN_POINT ( 'NONE',  ( 41.64333658814960870, 144.7151871740940123, 38.42115945441014446 ) ) ;
#8855 = FACE_OUTER_BOUND ( 'NONE', #10457, .T. ) ;
#8856 = CARTESIAN_POINT ( 'NONE',  ( 43.01140435219951286, 106.1297705074273097, 38.86567161673127657 ) ) ;
#8857 = CARTESIAN_POINT ( 'NONE',  ( 35.69068542950036260, 86.46542255174357194, 7.577194441455407770 ) ) ;
#8858 = ORIENTED_EDGE ( 'NONE', *, *, #9429, .F. ) ;
#8859 = CARTESIAN_POINT ( 'NONE',  ( 64.66009251794113766, 101.8366349233107684, -0.5580327111990067701 ) ) ;
#8860 = ORIENTED_EDGE ( 'NONE', *, *, #17923, .F. ) ;
#8861 = PLANE ( 'NONE',  #4378 ) ;
#8862 = DIRECTION ( 'NONE',  ( 0.000000000000000000, 0.000000000000000000, 1.000000000000000000 ) ) ;
#8863 = CARTESIAN_POINT ( 'NONE',  ( 38.58424406990784661, 140.9651871740939555, 32.77220824515698183 ) ) ;
#8864 = CARTESIAN_POINT ( 'NONE',  ( 48.01140435219951996, 98.36049967264872862, 32.58608133808903773 ) ) ;
#8865 = CARTESIAN_POINT ( 'NONE',  ( 57.78275410301085913, 89.02518083909171764, -0.1607367497116551913 ) ) ;
#8866 = CARTESIAN_POINT ( 'NONE',  ( 38.96631938032478359, 61.01049967264874141, 37.14960608071593384 ) ) ;
#8867 = CARTESIAN_POINT ( 'NONE',  ( -141.4692556286852891, -166.1391397928655067, 52.90620854394536821 ) ) ;
#8868 = CARTESIAN_POINT ( 'NONE',  ( 43.01140435219951286, 144.5344580088726048, 39.21067981925356349 ) ) ;
#8869 = CARTESIAN_POINT ( 'NONE',  ( 9.616596702810701558, 112.3753283828585694, -5.161025107254184618 ) ) ;
#8870 = CARTESIAN_POINT ( 'NONE',  ( -134.9004869860375777, 755.4811543468929358, -19.99999999999996092 ) ) ;
#8871 = CONTEXT_DEPENDENT_SHAPE_REPRESENTATION ( #18444, #16073 ) ;
#8872 = VECTOR ( 'NONE', #11605, 1000.000000000000000 ) ;
#8873 = CARTESIAN_POINT ( 'NONE',  ( 39.42975644700377558, 84.07977050742732672, 31.60846029578754468 ) ) ;
#8874 = CARTESIAN_POINT ( 'NONE',  ( -151.4692556286852891, -173.6438272943107108, 39.74470866294723947 ) ) ;
#8875 = CARTESIAN_POINT ( 'NONE',  ( 38.58424406990785371, 81.26518717409399528, 35.64915139335015937 ) ) ;
#8876 = CARTESIAN_POINT ( 'NONE',  ( -154.5594255724347761, -171.0891397928654669, 40.14644641866476604 ) ) ;
#8877 = DIRECTION ( 'NONE',  ( 0.000000000000000000, 0.000000000000000000, 1.000000000000000000 ) ) ;
#8878 = ORIENTED_EDGE ( 'NONE', *, *, #11790, .T. ) ;
#8879 = CARTESIAN_POINT ( 'NONE',  ( 47.05648932407426344, 85.58445800887258770, 31.27175355779120025 ) ) ;
#8880 = CARTESIAN_POINT ( 'NONE',  ( 43.01140435219951286, 128.0344580088725479, 29.21067981925356705 ) ) ;
#8881 = CARTESIAN_POINT ( 'NONE',  ( 46.59305225739526435, 130.5797705074273267, 36.81289934271958941 ) ) ;
#8882 = CARTESIAN_POINT ( 'NONE',  ( 77.08865571979157494, 122.1823731668103221, -14.48986716664726870 ) ) ;
#8883 = ORIENTED_EDGE ( 'NONE', *, *, #13409, .F. ) ;
#8884 = SURFACE_SIDE_STYLE ('',( #7233 ) ) ;
#8885 = EDGE_LOOP ( 'NONE', ( #1473, #5844, #18307, #9332, #7433, #3406, #10717, #10721, #19853, #16558 ) ) ;
#8886 = CARTESIAN_POINT ( 'NONE',  ( 43.01140435219951286, 131.6297705074273381, 29.55568802177586463 ) ) ;
#8887 = EDGE_CURVE ( 'NONE', #7018, #20087, #8521, .T. ) ;
#8888 = VECTOR ( 'NONE', #486, 1000.000000000000000 ) ;
#8889 = AXIS2_PLACEMENT_3D ( 'NONE', #6678, #20333, #10197 ) ;
#8890 = CARTESIAN_POINT ( 'NONE',  ( -143.3790856849358306, -180.6891397928654612, 43.77915905869157598 ) ) ;
#8891 = AXIS2_PLACEMENT_3D ( 'NONE', #21113, #19550, #18112 ) ;
#8892 = DIRECTION ( 'NONE',  ( -0.8510798296367592108, -0.5250363069212118372, 0.000000000000000000 ) ) ;
#8893 = CARTESIAN_POINT ( 'NONE',  ( 116.4417310231185780, -126.9891397928655010, 49.65701158161629536 ) ) ;
#8894 =( NAMED_UNIT ( * ) PLANE_ANGLE_UNIT ( ) SI_UNIT ( $, .RADIAN. ) );
#8895 = EDGE_CURVE ( 'NONE', #10633, #10863, #18320, .T. ) ;
#8896 = CARTESIAN_POINT ( 'NONE',  ( 39.42975644700377558, 102.4151871740940010, 36.81289934271958941 ) ) ;
#8897 = CARTESIAN_POINT ( 'NONE',  ( 41.46631938032478359, 153.1104996726487570, 29.45539723777780239 ) ) ;
#8898 = CARTESIAN_POINT ( 'NONE',  ( 43.01140435219951996, 10.71049967264875491, 39.21067981925356349 ) ) ;
#8899 = CARTESIAN_POINT ( 'NONE',  ( -161.4692556286852607, -163.7130981290892464, 46.40781461928724383 ) ) ;
#8900 = CARTESIAN_POINT ( 'NONE',  ( 48.01140435219951996, 142.1344580088725991, 35.83527830041810347 ) ) ;
#8901 = CARTESIAN_POINT ( 'NONE',  ( 46.59305225739526435, 116.1797705074273210, 31.60846029578754468 ) ) ;
#8902 = CARTESIAN_POINT ( 'NONE',  ( 71.28213884770818254, 119.1643779896719764, -2.300315981272657240 ) ) ;
#8903 = CARTESIAN_POINT ( 'NONE',  ( 44.55648932407425633, 100.8844580088725849, 29.45539723777780239 ) ) ;
#8904 = CARTESIAN_POINT ( 'NONE',  ( 38.58424406990786082, 108.1151871740940038, 34.21067981925357060 ) ) ;
#8905 = VERTEX_POINT ( 'NONE', #1788 ) ;
#8906 = CARTESIAN_POINT ( 'NONE',  ( 43.01140435219951286, 63.53445800887256922, 39.21067981925356349 ) ) ;
#8907 = CARTESIAN_POINT ( 'NONE',  ( 53.88337135589062399, 152.3674195137575964, -9.803719146365084569 ) ) ;
#8908 = CARTESIAN_POINT ( 'NONE',  ( 59.83664469576316236, 97.27638873328486113, 6.703993115985443119 ) ) ;
#8909 = FACE_OUTER_BOUND ( 'NONE', #2436, .T. ) ;
#8910 = CARTESIAN_POINT ( 'NONE',  ( 39.42975644700377558, 90.07977050742732672, 31.60846029578754468 ) ) ;
#8911 = ORIENTED_EDGE ( 'NONE', *, *, #11810, .F. ) ;
#8912 = CARTESIAN_POINT ( 'NONE',  ( 46.10157429594899270, 61.73445800887257917, 29.95742577749337343 ) ) ;
#8913 = DIRECTION ( 'NONE',  ( 0.000000000000000000, 1.000000000000000000, 0.000000000000000000 ) ) ;
#8914 = CARTESIAN_POINT ( 'NONE',  ( 39.92123440845004723, 132.2604996726487627, 29.95742577749337343 ) ) ;
#8915 = CARTESIAN_POINT ( 'NONE',  ( 44.37947211624943833, 86.21518717409399812, 30.00020018409699318 ) ) ;
#8916 = EDGE_CURVE ( 'NONE', #14655, #13351, #3291, .T. ) ;
#8917 = CARTESIAN_POINT ( 'NONE',  ( -157.2955611005346270, -160.7084106276440423, 57.67623309621198047 ) ) ;
#8918 = CARTESIAN_POINT ( 'NONE',  ( -154.3824083646099439, -185.4938272943107336, 40.69124936498395328 ) ) ;
#8919 = CARTESIAN_POINT ( 'NONE',  ( 111.4021762516569964, 137.5714195593754710, -35.00000000000000000 ) ) ;
#8920 = FACE_OUTER_BOUND ( 'NONE', #8041, .T. ) ;
#8921 = CARTESIAN_POINT ( 'NONE',  ( 46.10157429594899270, 143.6604996726487400, 29.95742577749336988 ) ) ;
#8922 = CARTESIAN_POINT ( 'NONE',  ( 40.27526882409969033, 140.9297705074273210, 30.44471234641811819 ) ) ;
#8923 = CARTESIAN_POINT ( 'NONE',  ( 47.43856463449117200, 106.7297705074273324, 35.64915139335016647 ) ) ;
#8924 = CARTESIAN_POINT ( 'NONE',  ( 62.84376099716368458, 92.00366499689042143, 13.64888190966157566 ) ) ;
#8925 = CARTESIAN_POINT ( 'NONE',  ( 39.42975644700377558, 135.4151871740940010, 36.81289934271958941 ) ) ;
#8926 = CARTESIAN_POINT ( 'NONE',  ( -145.6429501568359797, -155.9438272943106938, 41.63779006702063867 ) ) ;
#8927 = CARTESIAN_POINT ( 'NONE',  ( -148.5561028927606344, -162.0584106276440366, 40.69124936498395328 ) ) ;
#8928 = CARTESIAN_POINT ( 'NONE',  ( 43.01140435219951286, 62.62977050742732388, 29.55568802177586463 ) ) ;
#8929 = CARTESIAN_POINT ( 'NONE',  ( 43.01140435219951286, 92.03445800887257633, 29.21067981925356705 ) ) ;
#8930 = CARTESIAN_POINT ( 'NONE',  ( 24.55476856798156859, 141.3345980244743885, 9.128255474432329208 ) ) ;
#8931 = CARTESIAN_POINT ( 'NONE',  ( 141.4773229304660447, 84.89323405393692212, 14.00000000000001776 ) ) ;
#8932 = CARTESIAN_POINT ( 'NONE',  ( 38.58424406990784661, 110.9651871740940123, 32.77220824515698183 ) ) ;
#8933 = EDGE_LOOP ( 'NONE', ( #11196, #15122, #816, #15559 ) ) ;
#8934 = PLANE ( 'NONE',  #19093 ) ;
#8935 = ORIENTED_EDGE ( 'NONE', *, *, #11384, .T. ) ;
#8936 = ADVANCED_FACE ( 'NONE', ( #18090 ), #6417, .T. ) ;
#8937 = CARTESIAN_POINT ( 'NONE',  ( 43.01140435219951286, 99.53445800887259054, 39.46799094044489209 ) ) ;
#8938 = CARTESIAN_POINT ( 'NONE',  ( 38.58424406990785371, 147.2297705074273324, 32.77220824515697473 ) ) ;
#8939 = CARTESIAN_POINT ( 'NONE',  ( 38.01140435219952707, 159.7104996726487514, 34.21067981925357060 ) ) ;
#8941 = CARTESIAN_POINT ( 'NONE',  ( 67.15412698936957270, 134.4792784496449087, 12.06138812558265805 ) ) ;
#8940 = CARTESIAN_POINT ( 'NONE',  ( 43.01140435219951286, 117.8651871740939754, 38.86567161673127657 ) ) ;
#8942 = CARTESIAN_POINT ( 'NONE',  ( 38.01140435219951996, 75.86049967264874283, 35.83527830041810347 ) ) ;
#8944 = CARTESIAN_POINT ( 'NONE',  ( 46.10157429594899270, 135.8344580088725877, 38.46393386101375711 ) ) ;
#8943 = CARTESIAN_POINT ( 'NONE',  ( -158.9748091281504401, -126.9891397928655010, 62.65701158161630957 ) ) ;
#8945 = LINE ( 'NONE', #3766, #4028 ) ;
#8946 = CARTESIAN_POINT ( 'NONE',  ( 43.01140435219951996, 10.71049967264875491, 34.21067981925357060 ) ) ;
#8947 = CARTESIAN_POINT ( 'NONE',  ( 45.74753988029933538, 68.06518717409397823, 30.44471234641811819 ) ) ;
#8948 = FACE_OUTER_BOUND ( 'NONE', #19887, .T. ) ;
#8949 = CARTESIAN_POINT ( 'NONE',  ( -160.8964159109769696, -181.7438272943107336, 52.72008163687743121 ) ) ;
#8950 = CARTESIAN_POINT ( 'NONE',  ( -148.5561028927606344, -192.0584106276440650, 40.69124936498395328 ) ) ;
#8951 = ORIENTED_EDGE ( 'NONE', *, *, #661, .F. ) ;
#8952 =( BOUNDED_CURVE ( )  B_SPLINE_CURVE ( 2, ( #5170, #3632, #10355, #17058, #1970, #8704, #529, #15424, #319, #13754, #20494, #5383, #12099 ),
 .UNSPECIFIED., .F., .F. ) 
 B_SPLINE_CURVE_WITH_KNOTS ( ( 3, 2, 2, 2, 2, 2, 3 ),
 ( 0.4107142857142857539, 0.4142857142857143127, 0.4214285714285714302, 0.4285714285714285476, 0.4357142857142857206, 0.4428571428571428381, 0.4464285714285714524 ),
 .UNSPECIFIED. ) 
 CURVE ( )  GEOMETRIC_REPRESENTATION_ITEM ( )  RATIONAL_B_SPLINE_CURVE ( ( 0.9755282581475768211, 0.9755282581475769321, 1.000000000000000000, 0.9510565162951535312, 1.000000000000000000, 0.9510565162951535312, 1.000000000000000000, 0.9510565162951535312, 1.000000000000000000, 0.9510565162951535312, 1.000000000000000000, 0.9755282581475765991, 0.9755282581475768211 ) ) 
 REPRESENTATION_ITEM ( '' )  );
#8953 = CARTESIAN_POINT ( 'NONE',  ( -159.0959885057557983, -176.4584106276440707, 44.11586579668791330 ) ) ;
#8954 = CARTESIAN_POINT ( 'NONE',  ( 15.20278999188385960, 140.0102622722330636, 1.787054806504753346 ) ) ;
#8955 = ORIENTED_EDGE ( 'NONE', *, *, #13552, .T. ) ;
#8956 = CARTESIAN_POINT ( 'NONE',  ( 47.43856463449117200, 142.7651871740939669, 32.77220824515698183 ) ) ;
#8957 = PLANE ( 'NONE',  #8534 ) ;
#8958 = CARTESIAN_POINT ( 'NONE',  ( 38.58424406990785371, 102.2297705074273324, 32.77220824515697473 ) ) ;
#8959 = CARTESIAN_POINT ( 'NONE',  ( 71.03835150376274044, 100.2492380157770526, 6.267546321443639989 ) ) ;
#8960 = EDGE_LOOP ( 'NONE', ( #17910, #9586, #14470, #6603, #3933, #13236, #15986, #20451 ) ) ;
#8961 = CARTESIAN_POINT ( 'NONE',  ( 15.38454125381035098, 114.2504036285165654, 1.942219256913226388 ) ) ;
#8962 = ORIENTED_EDGE ( 'NONE', *, *, #17049, .T. ) ;
#8963 = EDGE_CURVE ( 'NONE', #1305, #9506, #17520, .T. ) ;
#8964 = AXIS2_PLACEMENT_3D ( 'NONE', #7324, #7535, #19211 ) ;
#8965 = CARTESIAN_POINT ( 'NONE',  ( 38.01140435219952707, 131.6344580088725706, 32.58608133808903773 ) ) ;
#8966 = LINE ( 'NONE', #15672, #6931 ) ;
#8967 = CARTESIAN_POINT ( 'NONE',  ( 45.74753988029933538, 82.42977050742732104, 37.97664729208901946 ) ) ;
#8968 = CARTESIAN_POINT ( 'NONE',  ( 46.59305225739526435, 145.9151871740940294, 31.60846029578754468 ) ) ;
#8969 = STYLED_ITEM ( 'NONE', ( #14519 ), #7648 ) ;
#8970 = CARTESIAN_POINT ( 'NONE',  ( 43.01140435219951286, 103.4604996726487087, 39.46799094044489209 ) ) ;
#8971 = CARTESIAN_POINT ( 'NONE',  ( 36.55618291757107841, 153.5264344809625641, -3.375052104409746789 ) ) ;
#8972 = CARTESIAN_POINT ( 'NONE',  ( 136.2768881589198884, 181.8432453435730167, 21.73429951086134082 ) ) ;
#8973 = CARTESIAN_POINT ( 'NONE',  ( -145.2889157411863721, -171.5391397928654555, 41.15050349809590102 ) ) ;
#8974 = CARTESIAN_POINT ( 'NONE',  ( -149.8854112254399240, -159.7362167067690280, 59.65701158161632378 ) ) ;
#8975 = CARTESIAN_POINT ( 'NONE',  ( 38.01140435219952707, 143.7844580088725763, 34.21067981925357060 ) ) ;
#8976 = CARTESIAN_POINT ( 'NONE',  ( -143.9637021292201950, -116.9891397928655010, 62.65701158161630957 ) ) ;
#8977 = ORIENTED_EDGE ( 'NONE', *, *, #16333, .T. ) ;
#8978 = CARTESIAN_POINT ( 'NONE',  ( 44.37947211624943833, 85.27977050742731535, 38.42115945441014446 ) ) ;
#8979 = CARTESIAN_POINT ( 'NONE',  ( -142.0420953463935803, -165.2438272943107052, 46.59394152635518793 ) ) ;
#8980 = CARTESIAN_POINT ( 'NONE',  ( 45.74753988029934249, 80.06518717409397823, 30.44471234641812174 ) ) ;
#8981 = CARTESIAN_POINT ( 'NONE',  ( 77.15313604554262383, 122.4041478163663612, -8.494263314424808087 ) ) ;
#8982 = CARTESIAN_POINT ( 'NONE',  ( -91.10645082872859746, 10.96617311717548660, 4.000000000000021316 ) ) ;
#8983 = VERTEX_POINT ( 'NONE', #133 ) ;
#8984 = EDGE_CURVE ( 'NONE', #12361, #13462, #3221, .T. ) ;
#8985 = CARTESIAN_POINT ( 'NONE',  ( 38.01140435219952707, 117.7104996726487371, 34.21067981925357060 ) ) ;
#8986 = CARTESIAN_POINT ( 'NONE',  ( -143.9637021292202235, -126.9891397928655010, 36.65701158161628825 ) ) ;
#8987 = CARTESIAN_POINT ( 'NONE',  ( 40.27526882409969744, 128.9297705074272926, 30.44471234641812174 ) ) ;
#8988 = CARTESIAN_POINT ( 'NONE',  ( 63.64508858465791974, 100.8029030738736225, 7.494358438614500351 ) ) ;
#8989 = EDGE_LOOP ( 'NONE', ( #2624, #12791 ) ) ;
#8990 = DIRECTION ( 'NONE',  ( -0.000000000000000000, -0.000000000000000000, -1.000000000000000000 ) ) ;
#8991 = ORIENTED_EDGE ( 'NONE', *, *, #5935, .T. ) ;
#8992 = CARTESIAN_POINT ( 'NONE',  ( 46.59305225739526435, 140.1797705074273210, 31.60846029578754468 ) ) ;
#8993 = CARTESIAN_POINT ( 'NONE',  ( 41.64333658814960870, 90.97977050742731819, 38.42115945441014446 ) ) ;
#8994 = CARTESIAN_POINT ( 'NONE',  ( -176.9699209214867608, -126.9891397928655010, 67.64809332337415526 ) ) ;
#8995 = CARTESIAN_POINT ( 'NONE',  ( 43.01140435219951286, 111.5344580088725905, 39.21067981925356349 ) ) ;
#8996 = CARTESIAN_POINT ( 'NONE',  ( 46.10157429594899270, 120.8344580088725593, 38.46393386101375711 ) ) ;
#8997 = CARTESIAN_POINT ( 'NONE',  ( -141.4692556286852891, -194.9130981290892635, 46.40781461928724383 ) ) ;
#8998 = CARTESIAN_POINT ( 'NONE',  ( 43.01140435219951286, 96.86518717409398960, 38.86567161673127657 ) ) ;
#8999 = CARTESIAN_POINT ( 'NONE',  ( -145.2889157411863437, -174.5130981290893146, 58.16351966513671812 ) ) ;
#9000 = CARTESIAN_POINT ( 'NONE',  ( -148.3790856849358306, -161.4630981290893317, 40.14644641866477315 ) ) ;
#9001 = DIRECTION ( 'NONE',  ( 1.000000000000000000, 0.000000000000000000, 0.000000000000000000 ) ) ;
#9002 = VECTOR ( 'NONE', #4155, 1000.000000000000000 ) ;
#9003 = CARTESIAN_POINT ( 'NONE',  ( 48.01140435219951996, 71.06049967264873146, 35.83527830041809636 ) ) ;
#9004 = CARTESIAN_POINT ( 'NONE',  ( 38.01140435219952707, 131.7844580088725763, 34.21067981925357060 ) ) ;
#9005 = CARTESIAN_POINT ( 'NONE',  ( 46.59305225739526435, 113.1797705074273210, 31.60846029578754468 ) ) ;
#9006 = CARTESIAN_POINT ( 'NONE',  ( 60.05828665636081354, 97.34093765924853869, 12.69960079420514809 ) ) ;
#9007 = CARTESIAN_POINT ( 'NONE',  ( -142.0420953463936087, -192.3938272943107393, 49.65701158161630957 ) ) ;
#9008 = CARTESIAN_POINT ( 'NONE',  ( 38.58424406990785371, 105.2651871740939953, 35.64915139335015937 ) ) ;
#9009 = ORIENTED_EDGE ( 'NONE', *, *, #1004, .T. ) ;
#9010 = EDGE_CURVE ( 'NONE', #15098, #15137, #4872, .T. ) ;
#9011 = CARTESIAN_POINT ( 'NONE',  ( 44.55648932407425633, 76.88445800887257064, 29.45539723777780239 ) ) ;
#9012 = CARTESIAN_POINT ( 'NONE',  ( 13.69124840528610321, 102.2378096837820181, -5.517995706778950016 ) ) ;
#9013 = CARTESIAN_POINT ( 'NONE',  ( 45.98873144221455789, 91.86516812052268222, 7.299390993452533394 ) ) ;
#9014 = CARTESIAN_POINT ( 'NONE',  ( 27.25521010731993243, 314.3399865783788414, -3.999999999999980904 ) ) ;
#9015 = CARTESIAN_POINT ( 'NONE',  ( 41.64333658814960870, 77.77977050742731535, 30.00020018409699318 ) ) ;
#9016 = ORIENTED_EDGE ( 'NONE', *, *, #11936, .T. ) ;
#9017 = VECTOR ( 'NONE', #20520, 1000.000000000000000 ) ;
#9018 = CARTESIAN_POINT ( 'NONE',  ( 43.01140435219951286, 68.03445800887259054, 28.95336869806222779 ) ) ;
#9019 = DIRECTION ( 'NONE',  ( 0.000000000000000000, -1.000000000000000000, 0.000000000000000000 ) ) ;
#9020 = AXIS2_PLACEMENT_3D ( 'NONE', #13568, #6531, #1569 ) ;
#9021 = CARTESIAN_POINT ( 'NONE',  ( 43.01140435219951286, 122.9604996726487371, 28.95336869806222779 ) ) ;
#9023 = CARTESIAN_POINT ( 'NONE',  ( 69.07271358049158039, 97.83220508185358710, -6.632443479277712051 ) ) ;
#9022 = CARTESIAN_POINT ( 'NONE',  ( 38.58424406990784661, 74.96518717409401233, 32.77220824515698183 ) ) ;
#9024 = CARTESIAN_POINT ( 'NONE',  ( -151.4692556286852891, -178.1438272943106824, 59.56931450028537256 ) ) ;
#9025 = CARTESIAN_POINT ( 'NONE',  ( 43.01140435219954838, 109.4604996726487371, 39.21067981925356349 ) ) ;
#9026 = CARTESIAN_POINT ( 'NONE',  ( -148.3790856849358306, -192.6630981290892919, 59.16757674456786020 ) ) ;
#9027 = CARTESIAN_POINT ( 'NONE',  ( 43.01140435219951286, 81.53445800887257633, 39.21067981925356349 ) ) ;
#9028 = FACE_BOUND ( 'NONE', #147, .T. ) ;
#9029 = CARTESIAN_POINT ( 'NONE',  ( 38.01140435219951996, 158.6344580088725706, 32.58608133808903773 ) ) ;
#9030 = CARTESIAN_POINT ( 'NONE',  ( 45.74753988029933538, 145.4297705074273210, 37.97664729208901946 ) ) ;
#9031 = CARTESIAN_POINT ( 'NONE',  ( 39.42975644700377558, 108.6797705074273352, 36.81289934271958941 ) ) ;
#9032 = CARTESIAN_POINT ( 'NONE',  ( 41.61242760320212852, 154.1118385459532760, 10.79173905232880237 ) ) ;
#9033 = CARTESIAN_POINT ( 'NONE',  ( 45.74753988029934249, 137.0651871740940067, 30.44471234641812174 ) ) ;
#9034 = AXIS2_PLACEMENT_3D ( 'NONE', #1316, #6272, #18059 ) ;
#9035 = CARTESIAN_POINT ( 'NONE',  ( -159.5594255724347761, -188.1891397928654612, 55.53486410454104316 ) ) ;
#9036 = CARTESIAN_POINT ( 'NONE',  ( -159.0959885057557983, -169.8584106276440764, 55.19815736654470584 ) ) ;
#9037 = CARTESIAN_POINT ( 'NONE',  ( 43.01140435219951996, 10.71049967264875491, 34.21067981925357060 ) ) ;
#9038 = AXIS2_PLACEMENT_3D ( 'NONE', #1477, #1253, #18227 ) ;
#9039 = DIRECTION ( 'NONE',  ( 0.4683024526015100442, -0.8835682276357669229, 0.000000000000000000 ) ) ;
#9040 = CARTESIAN_POINT ( 'NONE',  ( 70.99289463508769416, 124.0080672713295087, 11.50917073501047483 ) ) ;
#9041 = CYLINDRICAL_SURFACE ( 'NONE', #19036, 4.999999999999997335 ) ;
#9042 = CARTESIAN_POINT ( 'NONE',  ( 46.59305225739526435, 115.9151871740940010, 31.60846029578754468 ) ) ;
#9043 = EDGE_LOOP ( 'NONE', ( #14773, #9421, #21626, #16616 ) ) ;
#9044 = CARTESIAN_POINT ( 'NONE',  ( -154.5594255724347761, -180.0891397928654669, 40.14644641866476604 ) ) ;
#9045 = ORIENTED_EDGE ( 'NONE', *, *, #10967, .F. ) ;
#9046 = CARTESIAN_POINT ( 'NONE',  ( 38.96631938032478359, 89.48445800887257917, 31.27175355779120025 ) ) ;
#9047 = CARTESIAN_POINT ( 'NONE',  ( 41.64333658814960870, 150.9797705074273324, 38.42115945441014446 ) ) ;
#9048 = CARTESIAN_POINT ( 'NONE',  ( 41.46631938032478359, 159.1104996726487570, 29.45539723777780239 ) ) ;
#9050 = CARTESIAN_POINT ( 'NONE',  ( 29.95680074317227692, 144.8134228754239530, -2.624813489111333720 ) ) ;
#9049 = CARTESIAN_POINT ( 'NONE',  ( 38.58424406990784661, 111.2651871740939811, 35.64915139335016647 ) ) ;
#9051 = CARTESIAN_POINT ( 'NONE',  ( 38.01140435219952707, 75.71049967264873715, 34.21067981925357060 ) ) ;
#9053 = CARTESIAN_POINT ( 'NONE',  ( 43.01140435219951996, 149.0344580088725763, 29.21067981925357060 ) ) ;
#9052 = CARTESIAN_POINT ( 'NONE',  ( 39.92123440845005433, 108.2344580088725792, 38.46393386101375711 ) ) ;
#9054 = SURFACE_STYLE_USAGE ( .BOTH. , #2534 ) ;
#9055 = DIRECTION ( 'NONE',  ( 0.000000000000000000, -1.000000000000000000, 0.000000000000000000 ) ) ;
#9056 = FACE_OUTER_BOUND ( 'NONE', #9615, .T. ) ;
#9057 = CARTESIAN_POINT ( 'NONE',  ( 47.43856463449118621, 67.61518717409398960, 34.21067981925357060 ) ) ;
#9058 = CARTESIAN_POINT ( 'NONE',  ( 48.01140435219951996, 104.3604996726487428, 32.58608133808903773 ) ) ;
#9059 = CARTESIAN_POINT ( 'NONE',  ( -154.3824083646099439, -181.2938272943107449, 58.62277379824867296 ) ) ;
#9060 = CARTESIAN_POINT ( 'NONE',  ( -145.6429501568359797, -190.1084106276440195, 57.67623309621197336 ) ) ;
#9061 = ORIENTED_EDGE ( 'NONE', *, *, #4121, .F. ) ;
#9062 = CARTESIAN_POINT ( 'NONE',  ( -148.5561028927606344, -175.2584106276440536, 58.62277379824867296 ) ) ;
#9063 = VECTOR ( 'NONE', #21548, 1000.000000000000000 ) ;
#9064 = CARTESIAN_POINT ( 'NONE',  ( 10.28555834757860055, 130.2242880576791890, 1.430031502841225821 ) ) ;
#9065 = FACE_OUTER_BOUND ( 'NONE', #19114, .T. ) ;
#9066 = CARTESIAN_POINT ( 'NONE',  ( 41.64333658814960870, 143.5151871740939953, 30.00020018409699318 ) ) ;
#9067 = EDGE_CURVE ( 'NONE', #11702, #1696, #5497, .T. ) ;
#9068 = CARTESIAN_POINT ( 'NONE',  ( 47.43856463449117911, 104.0297705074273011, 32.77220824515697473 ) ) ;
#9069 = VERTEX_POINT ( 'NONE', #21 ) ;
#9070 = ORIENTED_EDGE ( 'NONE', *, *, #7748, .F. ) ;
#9071 = CARTESIAN_POINT ( 'NONE',  ( 31.84750084766683287, 94.01163676417708359, 0.8705387173494113506 ) ) ;
#9072 = EDGE_LOOP ( 'NONE', ( #21703, #10833, #2007, #925 ) ) ;
#9073 = CARTESIAN_POINT ( 'NONE',  ( 41.46631938032478359, 114.3844580088725849, 38.96596240072933170 ) ) ;
#9074 = CIRCLE ( 'NONE', #15751, 10.00000000000000888 ) ;
#9075 = CARTESIAN_POINT ( 'NONE',  ( 38.96631938032478359, 75.41049967264873999, 31.27175355779120025 ) ) ;
#9076 = CARTESIAN_POINT ( 'NONE',  ( 46.59305225739526435, 145.3151871740940067, 36.81289934271958941 ) ) ;
#9077 = CARTESIAN_POINT ( 'NONE',  ( 38.96631938032478359, 99.41049967264873999, 31.27175355779120025 ) ) ;
#9078 = CARTESIAN_POINT ( 'NONE',  ( 71.53613896966024299, 138.8348963267899592, -2.065403804986401859 ) ) ;
#9079 = ADVANCED_FACE ( 'NONE', ( #11369 ), #6862, .T. ) ;
#9080 = DIRECTION ( 'NONE',  ( 0.000000000000000000, 0.000000000000000000, 1.000000000000000000 ) ) ;
#9081 = CARTESIAN_POINT ( 'NONE',  ( -159.5594255724347761, -167.1891397928654897, 55.53486410454104316 ) ) ;
#9082 =( BOUNDED_CURVE ( )  B_SPLINE_CURVE ( 2, ( #1758, #18945, #3845, #8813, #20600, #5384, #5485, #7268, #8493, #15202, #2185, #12210, #105 ),
 .UNSPECIFIED., .F., .F. ) 
 B_SPLINE_CURVE_WITH_KNOTS ( ( 3, 2, 2, 2, 2, 2, 3 ),
 ( 0.3014705882352941013, 0.3029411764705882137, 0.3058823529411764941, 0.3088235294117647189, 0.3117647058823529438, 0.3147058823529411686, 0.3161764705882352811 ),
 .UNSPECIFIED. ) 
 CURVE ( )  GEOMETRIC_REPRESENTATION_ITEM ( )  RATIONAL_B_SPLINE_CURVE ( ( 0.9755282581475768211, 0.9755282581475768211, 1.000000000000000000, 0.9510565162951535312, 1.000000000000000000, 0.9510565162951535312, 1.000000000000000000, 0.9510565162951535312, 1.000000000000000000, 0.9510565162951535312, 1.000000000000000000, 0.9755282581475768211, 0.9755282581475768211 ) ) 
 REPRESENTATION_ITEM ( '' )  );
#9083 = DIRECTION ( 'NONE',  ( 1.000000000000000000, 0.000000000000000000, 0.000000000000000000 ) ) ;
#9084 = CARTESIAN_POINT ( 'NONE',  ( -151.4692556286852891, -196.9891397928655010, 39.65701158161630246 ) ) ;
#9085 = CARTESIAN_POINT ( 'NONE',  ( -166.4803626276155626, -126.9891397928655010, 49.65701158161629536 ) ) ;
#9086 = EDGE_CURVE ( 'NONE', #15220, #4183, #209, .T. ) ;
#9087 = ORIENTED_EDGE ( 'NONE', *, *, #5172, .T. ) ;
#9088 = CARTESIAN_POINT ( 'NONE',  ( 40.27526882409969033, 87.82977050742732672, 37.97664729208901946 ) ) ;
#9089 = CARTESIAN_POINT ( 'NONE',  ( -160.8964159109769696, -167.0438272943106881, 46.59394152635518793 ) ) ;
#9090 = EDGE_CURVE ( 'NONE', #10720, #13985, #1218, .T. ) ;
#9091 = CARTESIAN_POINT ( 'NONE',  ( 43.01140435219951286, 68.36518717409400381, 29.55568802177586107 ) ) ;
#9093 = VECTOR ( 'NONE', #9799, 1000.000000000000000 ) ;
#9092 = CARTESIAN_POINT ( 'NONE',  ( 71.14040157825178312, 139.4183699182763974, -9.089337262093875935 ) ) ;
#9094 = CARTESIAN_POINT ( 'NONE',  ( -151.4692556286852891, -194.9084106276440025, 39.74470866294723947 ) ) ;
#9095 = ORIENTED_EDGE ( 'NONE', *, *, #15940, .T. ) ;
#9096 = CARTESIAN_POINT ( 'NONE',  ( 42.21948215057684450, 117.0373810949690210, 29.21067981925356705 ) ) ;
#9097 = CARTESIAN_POINT ( 'NONE',  ( 43.01140435219951286, 122.9604996726487371, 29.21067981925356705 ) ) ;
#9098 = CARTESIAN_POINT ( 'NONE',  ( 44.37947211624943833, 133.2797705074273154, 38.42115945441014446 ) ) ;
#9099 = CARTESIAN_POINT ( 'NONE',  ( 36.14055301128134801, 147.1744539460121075, 4.637215583376333328 ) ) ;
#9100 = EDGE_CURVE ( 'NONE', #19943, #19802, #21527, .T. ) ;
#9101 = VERTEX_POINT ( 'NONE', #20098 ) ;
#9102 = DIRECTION ( 'NONE',  ( -0.9393725726208707050, -0.3428981916074316239, -0.000000000000000000 ) ) ;
#9103 = EDGE_LOOP ( 'NONE', ( #19441, #11957, #4579, #4974 ) ) ;
#9104 = CARTESIAN_POINT ( 'NONE',  ( 41.64333658814960870, 137.7797705074273154, 30.00020018409699318 ) ) ;
#9105 = CARTESIAN_POINT ( 'NONE',  ( 43.80332655382220253, 134.8836182503284817, 29.21067981925356705 ) ) ;
#9106 = ADVANCED_FACE ( 'NONE', ( #3332 ), #18433, .F. ) ;
#9107 = FACE_OUTER_BOUND ( 'NONE', #3695, .T. ) ;
#9108 = CARTESIAN_POINT ( 'NONE',  ( 47.05648932407426344, 121.5844580088725735, 31.27175355779120025 ) ) ;
#9109 =( NAMED_UNIT ( * ) SI_UNIT ( $, .STERADIAN. ) SOLID_ANGLE_UNIT ( ) );
#9110 = CARTESIAN_POINT ( 'NONE',  ( 41.64333658814960870, 95.51518717409400949, 30.00020018409699318 ) ) ;
#9111 = CARTESIAN_POINT ( 'NONE',  ( 38.96631938032478359, 66.41049967264873999, 31.27175355779120025 ) ) ;
#9112 = CARTESIAN_POINT ( 'NONE',  ( -91.10645082872859746, 10.96617311717548660, -19.99999999999997868 ) ) ;
#9113 = CARTESIAN_POINT ( 'NONE',  ( -148.3790856849358306, -155.4630981290893033, 40.14644641866477315 ) ) ;
#9114 = CARTESIAN_POINT ( 'NONE',  ( 0.000000000000000000, 0.000000000000000000, 0.000000000000000000 ) ) ;
#9115 = FACE_OUTER_BOUND ( 'NONE', #17452, .T. ) ;
#9116 = EDGE_CURVE ( 'NONE', #17048, #18846, #17863, .T. ) ;
#9117 = CARTESIAN_POINT ( 'NONE',  ( 38.96631938032478359, 128.4844580088725934, 31.27175355779120025 ) ) ;
#9118 = CARTESIAN_POINT ( 'NONE',  ( 38.58424406990784661, 117.5297705074273011, 35.64915139335016647 ) ) ;
#9119 = CARTESIAN_POINT ( 'NONE',  ( 64.86034851325717909, 101.9512479430583625, 5.437578391810254708 ) ) ;
#9120 = CARTESIAN_POINT ( 'NONE',  ( -151.4692556286852891, -190.1438272943107393, 59.56931450028537967 ) ) ;
#9121 = CARTESIAN_POINT ( 'NONE',  ( 40.27526882409969744, 98.66518717409400097, 30.44471234641812174 ) ) ;
#9122 = CARTESIAN_POINT ( 'NONE',  ( -141.4692556286852891, -161.9130981290893487, 46.40781461928724383 ) ) ;
#9123 = ORIENTED_EDGE ( 'NONE', *, *, #17267, .T. ) ;
#9124 = CARTESIAN_POINT ( 'NONE',  ( 61.61057083318216598, 91.16763906547615193, -7.303593892219363504 ) ) ;
#9125 = CARTESIAN_POINT ( 'NONE',  ( 15.96294818963569639, 111.9339314265907745, 8.846935114401974332 ) ) ;
#9126 = FACE_BOUND ( 'NONE', #7543, .T. ) ;
#9127 = CARTESIAN_POINT ( 'NONE',  ( 38.58424406990786082, 72.37977050742732388, 34.21067981925357060 ) ) ;
#9128 = ORIENTED_EDGE ( 'NONE', *, *, #9740, .T. ) ;
#9129 = ORIENTED_EDGE ( 'NONE', *, *, #20457, .T. ) ;
#9130 =( GEOMETRIC_REPRESENTATION_CONTEXT ( 3 ) GLOBAL_UNCERTAINTY_ASSIGNED_CONTEXT ( ( #11045 ) ) GLOBAL_UNIT_ASSIGNED_CONTEXT ( ( #21064, #19395, #21386 ) ) REPRESENTATION_CONTEXT ( 'NONE', 'WORKASPACE' ) );
#9131 = CIRCLE ( 'NONE', #4549, 27.58651506682278765 ) ;
#9132 = CARTESIAN_POINT ( 'NONE',  ( -151.4692556286853176, -164.3130981290893260, 39.65701158161629536 ) ) ;
#9133 = CARTESIAN_POINT ( 'NONE',  ( 48.01140435219951996, 116.0604996726487599, 35.83527830041810347 ) ) ;
#9135 = CARTESIAN_POINT ( 'NONE',  ( 30.47730968207189051, 151.6776658675815384, -2.585197649422186661 ) ) ;
#9134 = CARTESIAN_POINT ( 'NONE',  ( 45.74753988029933538, 82.16518717409400097, 37.97664729208901946 ) ) ;
#9136 = CARTESIAN_POINT ( 'NONE',  ( -143.8425227516148084, -168.6938272943107222, 55.19815736654470584 ) ) ;
#9137 = CARTESIAN_POINT ( 'NONE',  ( 68.29446192123552350, 96.82662215664792882, 13.41040346623746515 ) ) ;
#9138 = CARTESIAN_POINT ( 'NONE',  ( -161.4692556286852607, -184.7130981290893317, 46.40781461928724383 ) ) ;
#9139 = SHAPE_REPRESENTATION_RELATIONSHIP ( 'NONE' , 'NONE' ,  #5457, #2967 ) ;
#9140 = DIRECTION ( 'NONE',  ( 0.000000000000000000, 0.000000000000000000, 1.000000000000000000 ) ) ;
#9141 = CARTESIAN_POINT ( 'NONE',  ( 43.01140435219951286, 158.0344580088725763, 28.95336869806222779 ) ) ;
#9142 = CARTESIAN_POINT ( 'NONE',  ( 47.43856463449117200, 145.7297705074272756, 35.64915139335016647 ) ) ;
#9143 = CARTESIAN_POINT ( 'NONE',  ( 11.68597903420391226, 105.9017562933008918, 7.620467510411443435 ) ) ;
#9144 = CARTESIAN_POINT ( 'NONE',  ( 43.01140435219951286, 140.3651871740940180, 29.55568802177586107 ) ) ;
#9145 = CARTESIAN_POINT ( 'NONE',  ( 42.21948215057687293, 69.03738109496899256, 29.21067981925355994 ) ) ;
#9146 = CARTESIAN_POINT ( 'NONE',  ( -160.8964159109769696, -164.3084106276440650, 46.59394152635518083 ) ) ;
#9147 = VECTOR ( 'NONE', #13213, 1000.000000000000114 ) ;
#9148 = CARTESIAN_POINT ( 'NONE',  ( 38.58424406990786082, 60.37977050742732388, 34.21067981925357060 ) ) ;
#9149 = CARTESIAN_POINT ( 'NONE',  ( 107.0370895198517189, 343.6663954850758955, -3.999999999999996447 ) ) ;
#9150 =( BOUNDED_CURVE ( )  B_SPLINE_CURVE ( 2, ( #7886, #19894, #17890, #16020, #2803, #14701, #16243, #4783, #14374, #1151, #14587, #21330, #12946 ),
 .UNSPECIFIED., .F., .F. ) 
 B_SPLINE_CURVE_WITH_KNOTS ( ( 3, 2, 2, 2, 2, 2, 3 ),
 ( 0.4464285714285714524, 0.4500000000000000111, 0.4571428571428571286, 0.4642857142857143016, 0.4714285714285714191, 0.4785714285714285920, 0.4821428571428571508 ),
 .UNSPECIFIED. ) 
 CURVE ( )  GEOMETRIC_REPRESENTATION_ITEM ( )  RATIONAL_B_SPLINE_CURVE ( ( 0.9755282581475768211, 0.9755282581475769321, 1.000000000000000000, 0.9510565162951535312, 1.000000000000000000, 0.9510565162951535312, 1.000000000000000000, 0.9510565162951535312, 1.000000000000000000, 0.9510565162951535312, 1.000000000000000000, 0.9755282581475768211, 0.9755282581475768211 ) ) 
 REPRESENTATION_ITEM ( '' )  );
#9151 = CARTESIAN_POINT ( 'NONE',  ( 22.18708823908250238, 100.7722391081675255, 7.342430719951936524 ) ) ;
#9152 = CARTESIAN_POINT ( 'NONE',  ( 131.0765927465021434, 198.5836349573982886, 34.00000000000001421 ) ) ;
#9153 = CARTESIAN_POINT ( 'NONE',  ( 43.01140435219951286, 116.3651871740939896, 29.55568802177586463 ) ) ;
#9154 = ORIENTED_EDGE ( 'NONE', *, *, #3285, .F. ) ;
#9155 = CARTESIAN_POINT ( 'NONE',  ( -151.4692556286853176, -180.2391397928654726, 39.65701158161629536 ) ) ;
#9156 = EDGE_LOOP ( 'NONE', ( #6434, #4606 ) ) ;
#9157 = CARTESIAN_POINT ( 'NONE',  ( 38.96631938032478359, 96.08445800887258770, 37.14960608071593384 ) ) ;
#9158 = CARTESIAN_POINT ( 'NONE',  ( 40.27526882409969744, 147.8297705074272983, 37.97664729208901235 ) ) ;
#9159 = AXIS2_PLACEMENT_3D ( 'NONE', #7352, #17036, #19136 ) ;
#9160 = CARTESIAN_POINT ( 'NONE',  ( 46.10157429594899270, 152.6604996726487400, 29.95742577749337343 ) ) ;
#9162 = CARTESIAN_POINT ( 'NONE',  ( 15.65696388169908104, 126.4253507882334588, -3.577328847893908925 ) ) ;
#9161 = CARTESIAN_POINT ( 'NONE',  ( 43.01140435219951286, 102.8651871740940038, 38.86567161673127657 ) ) ;
#9163 = CARTESIAN_POINT ( 'NONE',  ( 43.01140435219951286, 59.96049967264874425, 28.95336869806222779 ) ) ;
#9165 = CARTESIAN_POINT ( 'NONE',  ( -148.3790856849358306, -183.6630981290893203, 59.16757674456786020 ) ) ;
#9164 = LINE ( 'NONE', #15863, #11500 ) ;
#9166 = FILL_AREA_STYLE_COLOUR ( '', #16112 ) ;
#9167 = FACE_BOUND ( 'NONE', #15105, .T. ) ;
#9168 = CARTESIAN_POINT ( 'NONE',  ( 111.4021762516569964, 137.5714195593754710, -35.00000000000000000 ) ) ;
#9169 = CARTESIAN_POINT ( 'NONE',  ( 44.37947211624943833, 67.01518717409399528, 38.42115945441014446 ) ) ;
#9170 = DIRECTION ( 'NONE',  ( -0.000000000000000000, -0.000000000000000000, 1.000000000000000000 ) ) ;
#9171 = CARTESIAN_POINT ( 'NONE',  ( -154.3824083646099439, -172.2938272943107165, 58.62277379824867296 ) ) ;
#9172 = CARTESIAN_POINT ( 'NONE',  ( -151.4692556286852891, -194.9084106276440025, 39.74470866294723947 ) ) ;
#9173 = ORIENTED_EDGE ( 'NONE', *, *, #1561, .F. ) ;
#9174 = CARTESIAN_POINT ( 'NONE',  ( 13.37233465371036090, 102.6159639102351093, 7.501340520787425525 ) ) ;
#9175 = ADVANCED_FACE ( 'NONE', ( #8624 ), #19084, .T. ) ;
#9176 = CARTESIAN_POINT ( 'NONE',  ( 157.5268905834513475, 193.0332408774651185, 14.00000000000001776 ) ) ;
#9177 = CARTESIAN_POINT ( 'NONE',  ( 43.01140435219951286, 144.8651871740939612, 38.86567161673127657 ) ) ;
#9178 = VECTOR ( 'NONE', #17963, 1000.000000000000000 ) ;
#9179 = CARTESIAN_POINT ( 'NONE',  ( 43.01140435219951286, 103.1297705074273097, 38.86567161673127657 ) ) ;
#9180 = ORIENTED_EDGE ( 'NONE', *, *, #4029, .F. ) ;
#9181 = ORIENTED_EDGE ( 'NONE', *, *, #21402, .F. ) ;
#9182 = CARTESIAN_POINT ( 'NONE',  ( 40.57367117788501787, 91.81261228707245436, 0.5136478283763052932 ) ) ;
#9183 = ORIENTED_EDGE ( 'NONE', *, *, #18437, .F. ) ;
#9184 = CARTESIAN_POINT ( 'NONE',  ( 39.92123440845004723, 114.2344580088725650, 38.46393386101376421 ) ) ;
#9185 = CARTESIAN_POINT ( 'NONE',  ( 91.17254549292282206, -61.68114226949890622, 10.00000000000001599 ) ) ;
#9186 = CARTESIAN_POINT ( 'NONE',  ( 45.74753988029933538, 74.32977050742729830, 30.44471234641811819 ) ) ;
#9187 = CARTESIAN_POINT ( 'NONE',  ( 43.01140435219951286, 138.8651871740940180, 38.86567161673127657 ) ) ;
#9188 = CARTESIAN_POINT ( 'NONE',  ( 48.01140435219951996, 104.2104996726487371, 34.21067981925357060 ) ) ;
#9189 = CARTESIAN_POINT ( 'NONE',  ( 76.40658810299491677, 127.4365358892444959, 12.33923360994393903 ) ) ;
#9190 = CARTESIAN_POINT ( 'NONE',  ( -148.3790856849358306, -180.6630981290893203, 59.16757674456786020 ) ) ;
#9191 = EDGE_CURVE ( 'NONE', #4997, #18531, #15172, .T. ) ;
#9192 = CARTESIAN_POINT ( 'NONE',  ( -143.3790856849358306, -160.2891397928654555, 55.53486410454105027 ) ) ;
#9193 = CARTESIAN_POINT ( 'NONE',  ( 42.21948215057684450, 153.4575765865523067, 39.21067981925356349 ) ) ;
#9194 = CARTESIAN_POINT ( 'NONE',  ( 38.01140435219952707, 143.9344580088725536, 35.83527830041809636 ) ) ;
#9195 = FACE_OUTER_BOUND ( 'NONE', #19280, .T. ) ;
#9196 = ORIENTED_EDGE ( 'NONE', *, *, #5620, .F. ) ;
#9197 = CARTESIAN_POINT ( 'NONE',  ( 43.01140435219951286, 88.12977050742732388, 38.86567161673127657 ) ) ;
#9198 = CARTESIAN_POINT ( 'NONE',  ( -148.5561028927606344, -165.9938272943107336, 58.62277379824867296 ) ) ;
#9199 = CARTESIAN_POINT ( 'NONE',  ( 9.616596702810701558, 112.3753283828585694, -5.161025107254184618 ) ) ;
#9200 = CARTESIAN_POINT ( 'NONE',  ( -154.3824083646099439, -191.7584106276440536, 40.69124936498395328 ) ) ;
#9201 = VERTEX_POINT ( 'NONE', #8845 ) ;
#9202 = CARTESIAN_POINT ( 'NONE',  ( -159.5594255724347761, -175.2630981290893146, 55.53486410454104316 ) ) ;
#9203 = CARTESIAN_POINT ( 'NONE',  ( 43.01140435219951286, 105.5344580088725621, 39.21067981925356349 ) ) ;
#9204 = CARTESIAN_POINT ( 'NONE',  ( 47.43856463449117911, 134.0297705074273154, 32.77220824515697473 ) ) ;
#9205 = CARTESIAN_POINT ( 'NONE',  ( 9.127117681521182746, 124.1904119534442401, -3.775300622140596030 ) ) ;
#9206 = ORIENTED_EDGE ( 'NONE', *, *, #4173, .F. ) ;
#9207 = ADVANCED_FACE ( 'NONE', ( #9056 ), #17195, .T. ) ;
#9208 = DIRECTION ( 'NONE',  ( 0.000000000000000000, 0.000000000000000000, 1.000000000000000000 ) ) ;
#9209 = EDGE_CURVE ( 'NONE', #120, #10393, #8393, .T. ) ;
#9210 = ORIENTED_EDGE ( 'NONE', *, *, #19040, .T. ) ;
#9211 = CARTESIAN_POINT ( 'NONE',  ( 47.43856463449117200, 128.0297705074273154, 32.77220824515698183 ) ) ;
#9212 = CARTESIAN_POINT ( 'NONE',  ( -39.63192160874135084, -354.7018910364275257, 20.00000000000002132 ) ) ;
#9213 =( BOUNDED_CURVE ( )  B_SPLINE_CURVE ( 2, ( #12157, #7218, #19214, #1130, #14894, #9844, #17979, #21530, #8081, #7865, #13034, #16544, #11477 ),
 .UNSPECIFIED., .F., .F. ) 
 B_SPLINE_CURVE_WITH_KNOTS ( ( 3, 2, 2, 2, 2, 2, 3 ),
 ( 0.06617647058823529493, 0.06764705882352940736, 0.07058823529411764608, 0.07352941176470588480, 0.07647058823529412352, 0.07941176470588234837, 0.08088235294117647467 ),
 .UNSPECIFIED. ) 
 CURVE ( )  GEOMETRIC_REPRESENTATION_ITEM ( )  RATIONAL_B_SPLINE_CURVE ( ( 0.9755282581475768211, 0.9755282581475768211, 1.000000000000000000, 0.9510565162951535312, 1.000000000000000000, 0.9510565162951535312, 1.000000000000000000, 0.9510565162951535312, 1.000000000000000000, 0.9510565162951535312, 1.000000000000000000, 0.9755282581475765991, 0.9755282581475767101 ) ) 
 REPRESENTATION_ITEM ( '' )  );
#9214 = EDGE_CURVE ( 'NONE', #19943, #21028, #16980, .T. ) ;
#9215 = CARTESIAN_POINT ( 'NONE',  ( 38.96631938032478359, 111.0844580088725735, 37.14960608071593384 ) ) ;
#9216 = CARTESIAN_POINT ( 'NONE',  ( 41.46631938032478359, 129.1104996726487570, 29.45539723777780239 ) ) ;
#9217 = CARTESIAN_POINT ( 'NONE',  ( -141.4692556286852891, -192.2130981290893033, 52.90620854394536821 ) ) ;
#9218 = CARTESIAN_POINT ( 'NONE',  ( 39.42975644700377558, 99.41518717409400097, 36.81289934271958941 ) ) ;
#9219 = CARTESIAN_POINT ( 'NONE',  ( 48.01140435219951996, 74.36049967264872862, 32.58608133808903773 ) ) ;
#9220 = LINE ( 'NONE', #3925, #900 ) ;
#9221 = CARTESIAN_POINT ( 'NONE',  ( -148.3790856849358306, -159.6630981290892919, 59.16757674456786020 ) ) ;
#9222 = DIRECTION ( 'NONE',  ( 0.000000000000000000, 0.000000000000000000, 1.000000000000000000 ) ) ;
#9223 = CARTESIAN_POINT ( 'NONE',  ( 41.46631938032478359, 132.3844580088725706, 38.96596240072933170 ) ) ;
#9224 = CARTESIAN_POINT ( 'NONE',  ( 38.96631938032478359, 135.0844580088725877, 37.14960608071593384 ) ) ;
#9225 = CARTESIAN_POINT ( 'NONE',  ( 47.43856463449117200, 112.7297705074273182, 35.64915139335016647 ) ) ;
#9226 = CARTESIAN_POINT ( 'NONE',  ( 14.87688376430095616, 117.0300574687981481, 8.056989239287382532 ) ) ;
#9227 = CARTESIAN_POINT ( 'NONE',  ( -154.3824083646099439, -191.4938272943107336, 40.69124936498395328 ) ) ;
#9228 = CARTESIAN_POINT ( 'NONE',  ( 44.37947211624943833, 94.01518717409400949, 38.42115945441014446 ) ) ;
#9229 = CARTESIAN_POINT ( 'NONE',  ( 43.01140435219951286, 89.03445800887257633, 29.21067981925356705 ) ) ;
#9230 = ORIENTED_EDGE ( 'NONE', *, *, #342, .T. ) ;
#9231 = CARTESIAN_POINT ( 'NONE',  ( -151.4692556286852607, -169.7391397928654442, 59.65701158161632378 ) ) ;
#9232 = CARTESIAN_POINT ( 'NONE',  ( 76.81974253126139729, 125.2811442093199616, -1.589308178208348910 ) ) ;
#9233 = CARTESIAN_POINT ( 'NONE',  ( 55.81398226145393693, 145.0329042473489096, 4.442248136324586483 ) ) ;
#9234 = CARTESIAN_POINT ( 'NONE',  ( -143.3790856849358306, -168.6891397928654897, 43.77915905869157598 ) ) ;
#9235 = AXIS2_PLACEMENT_3D ( 'NONE', #5107, #16669, #13482 ) ;
#9236 = CARTESIAN_POINT ( 'NONE',  ( 47.43856463449117911, 80.02977050742731535, 32.77220824515697473 ) ) ;
#9237 = ORIENTED_EDGE ( 'NONE', *, *, #15967, .F. ) ;
#9238 = ORIENTED_EDGE ( 'NONE', *, *, #6609, .F. ) ;
#9239 = CARTESIAN_POINT ( 'NONE',  ( 156.1725454929228079, -61.68114226949890622, -46.21320343559645494 ) ) ;
#9240 = AXIS2_PLACEMENT_3D ( 'NONE', #15914, #2579, #18911 ) ;
#9241 = FACE_BOUND ( 'NONE', #8989, .T. ) ;
#9242 = CARTESIAN_POINT ( 'NONE',  ( 47.05648932407426344, 122.5104996726487343, 31.27175355779120025 ) ) ;
#9244 = CARTESIAN_POINT ( 'NONE',  ( 63.19260820189420969, 92.35335041358771946, 0.6293402173502762320 ) ) ;
#9243 = CARTESIAN_POINT ( 'NONE',  ( 47.43856463449117200, 82.46518717409398391, 35.64915139335016647 ) ) ;
#9245 = CARTESIAN_POINT ( 'NONE',  ( -160.8964159109769696, -169.8938272943107393, 49.65701158161630957 ) ) ;
#9246 = CARTESIAN_POINT ( 'NONE',  ( -148.3790856849358306, -186.6630981290893203, 59.16757674456786020 ) ) ;
#9247 = VECTOR ( 'NONE', #8552, 1000.000000000000000 ) ;
#9248 = CARTESIAN_POINT ( 'NONE',  ( 31.20897972572539558, 148.4098837309084900, 17.43780275515693390 ) ) ;
#9249 = CARTESIAN_POINT ( 'NONE',  ( 48.01140435219951996, 157.1344580088725422, 35.83527830041810347 ) ) ;
#9250 = CARTESIAN_POINT ( 'NONE',  ( 46.59305225739526435, 140.1797705074273210, 31.60846029578754468 ) ) ;
#9251 = CARTESIAN_POINT ( 'NONE',  ( 30.25101221841200427, 88.05347211559326581, -0.2365872832861977970 ) ) ;
#9252 = CARTESIAN_POINT ( 'NONE',  ( 46.59305225739526435, 124.3151871740940067, 36.81289934271958941 ) ) ;
#9253 = CARTESIAN_POINT ( 'NONE',  ( -142.0420953463935803, -162.8084106276440650, 52.72008163687743831 ) ) ;
#9254 = CARTESIAN_POINT ( 'NONE',  ( 43.01140435219951286, 98.03445800887257633, 29.21067981925356705 ) ) ;
#9255 = CARTESIAN_POINT ( 'NONE',  ( 47.05648932407426344, 91.58445800887257349, 31.27175355779120025 ) ) ;
#9256 = CARTESIAN_POINT ( 'NONE',  ( 29.49905557571407044, 144.7517438296894738, 9.366394860000250233 ) ) ;
#9257 = CARTESIAN_POINT ( 'NONE',  ( 132.3486983259487886, 110.2203079035326851, -19.99999999999999645 ) ) ;
#9258 = CARTESIAN_POINT ( 'NONE',  ( 47.43856463449117200, 103.7651871740939669, 32.77220824515698183 ) ) ;
#9259 = EDGE_CURVE ( 'NONE', #6487, #12008, #20656, .T. ) ;
#9260 = ORIENTED_EDGE ( 'NONE', *, *, #12468, .T. ) ;
#9261 = LINE ( 'NONE', #21156, #18023 ) ;
#9262 = ORIENTED_EDGE ( 'NONE', *, *, #19692, .T. ) ;
#9263 = CARTESIAN_POINT ( 'NONE',  ( 48.01140435219951996, 91.13445800887257064, 35.83527830041810347 ) ) ;
#9264 = CARTESIAN_POINT ( 'NONE',  ( 48.01140435219951996, 149.2104996726487514, 34.21067981925357060 ) ) ;
#9266 = CARTESIAN_POINT ( 'NONE',  ( 52.67254683800726411, 146.3150465326280028, -8.696212858991016148 ) ) ;
#9265 = CARTESIAN_POINT ( 'NONE',  ( 39.42975644700377558, 110.8151871740939924, 31.60846029578754468 ) ) ;
#9267 = CARTESIAN_POINT ( 'NONE',  ( 38.01140435219951996, 66.56049967264871725, 32.58608133808903773 ) ) ;
#9269 = CARTESIAN_POINT ( 'NONE',  ( -157.6495955161842062, -158.0130981290893146, 41.15050349809589392 ) ) ;
#9268 = CARTESIAN_POINT ( 'NONE',  ( 47.50526184765048754, 144.5001958438514009, 36.42700876960374501 ) ) ;
#9270 =( NAMED_UNIT ( * ) PLANE_ANGLE_UNIT ( ) SI_UNIT ( $, .RADIAN. ) );
#9271 = CARTESIAN_POINT ( 'NONE',  ( 159.0505745212445561, 203.5296818892961994, 34.00000000000001421 ) ) ;
#9272 =( BOUNDED_CURVE ( )  B_SPLINE_CURVE ( 1, ( #14110, #12247 ),
 .UNSPECIFIED., .F., .F. ) 
 B_SPLINE_CURVE_WITH_KNOTS ( ( 2, 2 ),
 ( 0.000000000000000000, 1.000000000000000000 ),
 .UNSPECIFIED. ) 
 CURVE ( )  GEOMETRIC_REPRESENTATION_ITEM ( )  RATIONAL_B_SPLINE_CURVE ( ( 0.9782066976764471899, 0.9782066976764471899 ) ) 
 REPRESENTATION_ITEM ( '' )  );
#9273 = CARTESIAN_POINT ( 'NONE',  ( 40.27526882409969033, 69.56518717409400665, 37.97664729208901946 ) ) ;
#9274 = DIRECTION ( 'NONE',  ( -0.9393725726208707050, -0.3428981916074317349, 0.000000000000000000 ) ) ;
#9275 = DIRECTION ( 'NONE',  ( 0.000000000000000000, 0.000000000000000000, 1.000000000000000000 ) ) ;
#9276 = CARTESIAN_POINT ( 'NONE',  ( -142.0420953463935803, -168.2438272943107336, 46.59394152635518793 ) ) ;
#9277 = CARTESIAN_POINT ( 'NONE',  ( -159.0959885057557983, -190.8584106276440480, 55.19815736654470584 ) ) ;
#9278 = EDGE_LOOP ( 'NONE', ( #21569, #1804 ) ) ;
#9279 = CARTESIAN_POINT ( 'NONE',  ( -143.8425227516148084, -177.3584106276440480, 44.11586579668791330 ) ) ;
#9280 = CARTESIAN_POINT ( 'NONE',  ( 43.59077634914400079, 154.2158251336064723, 2.858602931426994953 ) ) ;
#9281 = VERTEX_POINT ( 'NONE', #5947 ) ;
#9282 = CARTESIAN_POINT ( 'NONE',  ( 43.01140435219951286, 129.8651871740940180, 38.86567161673127657 ) ) ;
#9283 = EDGE_CURVE ( 'NONE', #18391, #13378, #20702, .T. ) ;
#9284 = CARTESIAN_POINT ( 'NONE',  ( 47.43856463449117911, 98.02977050742731535, 32.77220824515697473 ) ) ;
#9285 = ORIENTED_EDGE ( 'NONE', *, *, #20323, .T. ) ;
#9286 = ORIENTED_EDGE ( 'NONE', *, *, #13492, .F. ) ;
#9287 = CARTESIAN_POINT ( 'NONE',  ( 24.77189431714078083, 141.4131305960171687, 3.132649400142189844 ) ) ;
#9288 = ORIENTED_EDGE ( 'NONE', *, *, #20512, .F. ) ;
#9289 = CARTESIAN_POINT ( 'NONE',  ( 48.01140435219951996, 112.2844580088725763, 34.21067981925357060 ) ) ;
#9290 = CARTESIAN_POINT ( 'NONE',  ( 41.46631938032478359, 75.11049967264874283, 29.45539723777780239 ) ) ;
#9291 = CARTESIAN_POINT ( 'NONE',  ( 44.37947211624943833, 76.27977050742731535, 38.42115945441014446 ) ) ;
#9292 = CARTESIAN_POINT ( 'NONE',  ( 40.27526882409969033, 135.5651871740939782, 37.97664729208901946 ) ) ;
#9293 = CARTESIAN_POINT ( 'NONE',  ( 44.55648932407425633, 95.81049967264873146, 29.45539723777780239 ) ) ;
#9294 = CARTESIAN_POINT ( 'NONE',  ( 21.43032318156618388, 146.4805633285969861, 10.07716523980869816 ) ) ;
#9295 = CARTESIAN_POINT ( 'NONE',  ( 39.24942077270426211, 95.19152545906743512, 37.50829531803063333 ) ) ;
#9296 = CARTESIAN_POINT ( 'NONE',  ( -141.4692556286852891, -156.8391397928654669, 46.40781461928724383 ) ) ;
#9297 = CARTESIAN_POINT ( 'NONE',  ( 148.6725454929228079, -61.68114226949890622, 30.00000000000000000 ) ) ;
#9298 = CARTESIAN_POINT ( 'NONE',  ( 138.4989748031516967, 208.9305787985672680, -44.99999999999997158 ) ) ;
#9299 = CIRCLE ( 'NONE', #17027, 10.00000000000000888 ) ;
#9300 = CYLINDRICAL_SURFACE ( 'NONE', #8177, 4.999999999999997335 ) ;
#9301 = ORIENTED_EDGE ( 'NONE', *, *, #15069, .T. ) ;
#9302 = CARTESIAN_POINT ( 'NONE',  ( 44.37947211624943833, 77.47977050742731819, 30.00020018409699318 ) ) ;
#9303 = CARTESIAN_POINT ( 'NONE',  ( -159.0959885057557983, -164.1938272943107222, 44.11586579668791330 ) ) ;
#9304 = CARTESIAN_POINT ( 'NONE',  ( 64.11693453485118255, 146.8606268255622638, -2.422805558527139080 ) ) ;
#9305 = CARTESIAN_POINT ( 'NONE',  ( 43.01140435219951996, 119.9070776186055838, 8.284271247461942878 ) ) ;
#9306 = EDGE_LOOP ( 'NONE', ( #15852, #7851, #15044, #8058 ) ) ;
#9307 = CARTESIAN_POINT ( 'NONE',  ( -136.6255475934131596, 760.1741454933652449, -19.99999999999996092 ) ) ;
#9308 = DIRECTION ( 'NONE',  ( 0.000000000000000000, 0.000000000000000000, -1.000000000000000000 ) ) ;
#9309 = AXIS2_PLACEMENT_3D ( 'NONE', #13782, #3983, #13890 ) ;
#9310 = CARTESIAN_POINT ( 'NONE',  ( 38.58424406990785371, 126.2297705074273182, 32.77220824515697473 ) ) ;
#9311 = ORIENTED_EDGE ( 'NONE', *, *, #4921, .T. ) ;
#9312 = DIRECTION ( 'NONE',  ( 1.000000000000000000, 0.000000000000000000, 0.000000000000000000 ) ) ;
#9313 = ORIENTED_EDGE ( 'NONE', *, *, #21546, .T. ) ;
#9314 = CARTESIAN_POINT ( 'NONE',  ( 46.59305225739526435, 127.5797705074273267, 36.81289934271958941 ) ) ;
#9315 = DIRECTION ( 'NONE',  ( -0.000000000000000000, 1.000000000000000000, -0.000000000000000000 ) ) ;
#9316 = CARTESIAN_POINT ( 'NONE',  ( 41.46631938032478359, 100.3104996726487457, 38.96596240072933170 ) ) ;
#9317 = CARTESIAN_POINT ( 'NONE',  ( 38.96631938032478359, 130.0104996726487343, 37.14960608071593384 ) ) ;
#9318 = CARTESIAN_POINT ( 'NONE',  ( 38.96631938032478359, 97.01049967264874851, 37.14960608071593384 ) ) ;
#9319 = CARTESIAN_POINT ( 'NONE',  ( -151.4692556286852891, -189.2391397928654158, 39.14238933923362396 ) ) ;
#9320 = ADVANCED_FACE ( 'NONE', ( #17951 ), #2857, .F. ) ;
#9321 = VECTOR ( 'NONE', #15920, 1000.000000000000000 ) ;
#9322 = DIRECTION ( 'NONE',  ( 0.000000000000000000, 1.000000000000000000, 0.000000000000000000 ) ) ;
#9323 = CARTESIAN_POINT ( 'NONE',  ( 43.80332655382220253, 125.8836182503284533, 29.21067981925356705 ) ) ;
#9324 = CARTESIAN_POINT ( 'NONE',  ( -159.5594255724347761, -160.8630981290893089, 43.77915905869157598 ) ) ;
#9325 = APPLICATION_PROTOCOL_DEFINITION ( 'draft international standard', 'automotive_design', 1998, #10431 ) ;
#9326 = CARTESIAN_POINT ( 'NONE',  ( 41.46631938032478359, 129.3844580088725706, 38.96596240072933170 ) ) ;
#9327 = CARTESIAN_POINT ( 'NONE',  ( 43.01140435219951286, 106.1297705074272955, 38.86567161673127657 ) ) ;
#9328 = CARTESIAN_POINT ( 'NONE',  ( 68.00896726847550156, 133.1338957242411709, 4.128172222816925085 ) ) ;
#9329 = CARTESIAN_POINT ( 'NONE',  ( -151.4692556286852891, -193.1438272943107393, 59.56931450028537967 ) ) ;
#9330 = CARTESIAN_POINT ( 'NONE',  ( 38.58424406990785371, 92.96518717409401233, 32.77220824515697473 ) ) ;
#9331 = DIRECTION ( 'NONE',  ( 0.000000000000000000, 0.000000000000000000, -1.000000000000000000 ) ) ;
#9332 = ORIENTED_EDGE ( 'NONE', *, *, #5345, .T. ) ;
#9333 = CARTESIAN_POINT ( 'NONE',  ( 50.92548328124963319, 86.60151408976496157, 0.07716523989554470442 ) ) ;
#9334 = CARTESIAN_POINT ( 'NONE',  ( 18.82712405543679779, 105.5606057458561793, -11.43438524559667790 ) ) ;
#9335 = CARTESIAN_POINT ( 'NONE',  ( 17.73005198514846725, 142.9879744078657779, -4.089424278207452801 ) ) ;
#9336 = CARTESIAN_POINT ( 'NONE',  ( 44.37947211624943833, 80.47977050742731819, 30.00020018409699318 ) ) ;
#9337 =( BOUNDED_CURVE ( )  B_SPLINE_CURVE ( 1, ( #8582, #1957 ),
 .UNSPECIFIED., .F., .F. ) 
 B_SPLINE_CURVE_WITH_KNOTS ( ( 2, 2 ),
 ( 0.000000000000000000, 1.000000000000000000 ),
 .UNSPECIFIED. ) 
 CURVE ( )  GEOMETRIC_REPRESENTATION_ITEM ( )  RATIONAL_B_SPLINE_CURVE ( ( 0.9782068950532306628, 0.9782068950532306628 ) ) 
 REPRESENTATION_ITEM ( '' )  );
#9338 = VERTEX_POINT ( 'NONE', #6057 ) ;
#9339 = ORIENTED_EDGE ( 'NONE', *, *, #17326, .F. ) ;
#9340 = CARTESIAN_POINT ( 'NONE',  ( 40.27526882409969033, 156.8297705074272983, 37.97664729208901946 ) ) ;
#9341 = CARTESIAN_POINT ( 'NONE',  ( 173.3794444120442222, -136.9891397928655010, 19.99999999999999645 ) ) ;
#9342 = VECTOR ( 'NONE', #9476, 1000.000000000000000 ) ;
#9343 = CARTESIAN_POINT ( 'NONE',  ( 39.92123440845004723, 117.2604996726487485, 29.95742577749337343 ) ) ;
#9345 = CARTESIAN_POINT ( 'NONE',  ( 9.504183449854689769, 113.2927979568517571, -4.132695447411913747 ) ) ;
#9344 = CARTESIAN_POINT ( 'NONE',  ( 44.37947211624943833, 79.01518717409400949, 38.42115945441014446 ) ) ;
#9346 = CARTESIAN_POINT ( 'NONE',  ( -142.0420953463935803, -174.2438272943107052, 46.59394152635518083 ) ) ;
#9347 = CARTESIAN_POINT ( 'NONE',  ( 48.01140435219951996, 113.2104996726487371, 34.21067981925357060 ) ) ;
#9348 = CARTESIAN_POINT ( 'NONE',  ( -145.2889157411863721, -191.6130981290893089, 41.15050349809590102 ) ) ;
#9349 = SHAPE_REPRESENTATION_RELATIONSHIP ( 'NONE' , 'NONE' ,  #21416, #10590 ) ;
#9350 = DIRECTION ( 'NONE',  ( 1.000000000000000000, 0.000000000000000000, -0.000000000000000000 ) ) ;
#9351 = CARTESIAN_POINT ( 'NONE',  ( 44.37947211624943833, 146.4797705074273324, 30.00020018409699318 ) ) ;
#9352 = CARTESIAN_POINT ( 'NONE',  ( 8.916504151126011024, 123.7798070670463773, 8.215921583872152212 ) ) ;
#9353 = CARTESIAN_POINT ( 'NONE',  ( 44.37947211624943833, 122.2151871740940123, 30.00020018409699318 ) ) ;
#9354 = CARTESIAN_POINT ( 'NONE',  ( 42.21948215057684450, 70.38361825032846752, 39.21067981925355639 ) ) ;
#9355 = CARTESIAN_POINT ( 'NONE',  ( -142.0420953463935803, -159.5084106276440252, 46.59394152635518083 ) ) ;
#9356 = EDGE_CURVE ( 'NONE', #8531, #9507, #2637, .T. ) ;
#9357 = CARTESIAN_POINT ( 'NONE',  ( 44.37947211624943833, 59.47977050742732530, 30.00020018409699318 ) ) ;
#9358 = CARTESIAN_POINT ( 'NONE',  ( 44.55648932407425633, 148.6104996726487570, 38.96596240072933170 ) ) ;
#9359 = EDGE_CURVE ( 'NONE', #7746, #1989, #4509, .T. ) ;
#9360 = CARTESIAN_POINT ( 'NONE',  ( 70.05982654948900290, 127.8813624167294023, -8.653178033719973072 ) ) ;
#9361 = AXIS2_PLACEMENT_3D ( 'NONE', #21226, #9544, #13166 ) ;
#9362 = CYLINDRICAL_SURFACE ( 'NONE', #16203, 24.99999999999998579 ) ;
#9363 = CARTESIAN_POINT ( 'NONE',  ( 39.42975644700377558, 108.4151871740940152, 36.81289934271958941 ) ) ;
#9364 = ORIENTED_EDGE ( 'NONE', *, *, #3466, .F. ) ;
#9365 = ORIENTED_EDGE ( 'NONE', *, *, #19858, .T. ) ;
#9366 = CARTESIAN_POINT ( 'NONE',  ( 48.01140435219951996, 88.13445800887258486, 35.83527830041810347 ) ) ;
#9367 = DIRECTION ( 'NONE',  ( 0.000000000000000000, 0.000000000000000000, 1.000000000000000000 ) ) ;
#9368 = VECTOR ( 'NONE', #14738, 1000.000000000000000 ) ;
#9369 = CARTESIAN_POINT ( 'NONE',  ( 38.01140435219951996, 150.8604996726487286, 35.83527830041810347 ) ) ;
#9371 = CARTESIAN_POINT ( 'NONE',  ( 24.58042389364637259, 98.66975071380154816, -11.79164420265881574 ) ) ;
#9370 = CARTESIAN_POINT ( 'NONE',  ( 38.58424406990784661, 101.9651871740939981, 32.77220824515698183 ) ) ;
#9372 = VECTOR ( 'NONE', #13820, 1000.000000000000000 ) ;
#9373 = CARTESIAN_POINT ( 'NONE',  ( 47.05648932407426344, 65.51049967264874851, 31.27175355779120025 ) ) ;
#9374 = CARTESIAN_POINT ( 'NONE',  ( 134.6380592378699532, 268.5785371414991687, -19.99999999999997868 ) ) ;
#9375 =( LENGTH_UNIT ( ) NAMED_UNIT ( * ) SI_UNIT ( .MILLI., .METRE. ) );
#9376 = CIRCLE ( 'NONE', #2672, 10.00000000000000888 ) ;
#9377 = CARTESIAN_POINT ( 'NONE',  ( 43.80332655382220253, 79.95757658655229250, 29.21067981925356705 ) ) ;
#9378 = DIRECTION ( 'NONE',  ( 0.000000000000000000, 0.000000000000000000, 1.000000000000000000 ) ) ;
#9379 = VECTOR ( 'NONE', #7122, 1000.000000000000000 ) ;
#9380 = CARTESIAN_POINT ( 'NONE',  ( 47.43856463449117200, 73.76518717409399528, 32.77220824515698183 ) ) ;
#9381 = DIRECTION ( 'NONE',  ( -0.000000000000000000, -0.000000000000000000, -1.000000000000000000 ) ) ;
#9382 = CARTESIAN_POINT ( 'NONE',  ( 43.01140435219951286, 153.8651871740939896, 38.86567161673127657 ) ) ;
#9383 = CARTESIAN_POINT ( 'NONE',  ( 43.80332655382220253, 95.88361825032846752, 29.21067981925356705 ) ) ;
#9384 = CARTESIAN_POINT ( 'NONE',  ( -160.8964159109769696, -175.7438272943107052, 52.72008163687743121 ) ) ;
#9385 = CARTESIAN_POINT ( 'NONE',  ( -154.3824083646099439, -181.5584106276440650, 58.62277379824867296 ) ) ;
#9386 = ORIENTED_EDGE ( 'NONE', *, *, #4507, .F. ) ;
#9387 = CARTESIAN_POINT ( 'NONE',  ( -159.0959885057557983, -172.8584106276440764, 55.19815736654470584 ) ) ;
#9388 = CARTESIAN_POINT ( 'NONE',  ( 22.95395889711706872, 147.7494453258605915, 2.144227187454380790 ) ) ;
#9389 = DIRECTION ( 'NONE',  ( 0.000000000000000000, 0.000000000000000000, 1.000000000000000000 ) ) ;
#9390 = CARTESIAN_POINT ( 'NONE',  ( 43.01140435219951286, 134.3651871740939612, 29.55568802177586463 ) ) ;
#9391 = CARTESIAN_POINT ( 'NONE',  ( 40.27526882409969744, 92.92977050742730682, 30.44471234641812174 ) ) ;
#9392 = VECTOR ( 'NONE', #7623, 1000.000000000000000 ) ;
#9393 = ORIENTED_EDGE ( 'NONE', *, *, #11753, .T. ) ;
#9394 = ORIENTED_EDGE ( 'NONE', *, *, #12584, .T. ) ;
#9395 = CARTESIAN_POINT ( 'NONE',  ( 41.83412315030695794, 148.0818998446914634, 10.87053871734362431 ) ) ;
#9396 = CIRCLE ( 'NONE', #12198, 44.28464465043163756 ) ;
#9397 = ORIENTED_EDGE ( 'NONE', *, *, #1934, .F. ) ;
#9398 = DIRECTION ( 'NONE',  ( 0.000000000000000000, 1.000000000000000000, 0.000000000000000000 ) ) ;
#9399 = CARTESIAN_POINT ( 'NONE',  ( 47.43856463449118621, 79.87977050742732388, 34.21067981925357060 ) ) ;
#9400 = CARTESIAN_POINT ( 'NONE',  ( 43.01140435219951286, 134.3651871740939612, 29.55568802177586463 ) ) ;
#9401 =( BOUNDED_CURVE ( )  B_SPLINE_CURVE ( 2, ( #12067, #5137, #16918, #5451, #11854, #286, #8457, #1830, #12170, #6803, #3492, #15390, #63 ),
 .UNSPECIFIED., .F., .F. ) 
 B_SPLINE_CURVE_WITH_KNOTS ( ( 3, 2, 2, 2, 2, 2, 3 ),
 ( 0.3750000000000000000, 0.3764705882352941124, 0.3794117647058823373, 0.3823529411764705621, 0.3852941176470588425, 0.3882352941176470673, 0.3897058823529411797 ),
 .UNSPECIFIED. ) 
 CURVE ( )  GEOMETRIC_REPRESENTATION_ITEM ( )  RATIONAL_B_SPLINE_CURVE ( ( 0.9755282581475768211, 0.9755282581475768211, 1.000000000000000000, 0.9510565162951535312, 1.000000000000000000, 0.9510565162951535312, 1.000000000000000000, 0.9510565162951535312, 1.000000000000000000, 0.9510565162951535312, 1.000000000000000000, 0.9755282581475768211, 0.9755282581475768211 ) ) 
 REPRESENTATION_ITEM ( '' )  );
#9402 = CARTESIAN_POINT ( 'NONE',  ( 47.05648932407426344, 88.91049967264873999, 37.14960608071593384 ) ) ;
#9403 = CARTESIAN_POINT ( 'NONE',  ( 25.52397925108762067, 90.47728371212039633, 7.934596195134201224 ) ) ;
#9404 = EDGE_CURVE ( 'NONE', #21213, #8340, #7941, .T. ) ;
#9405 = DIRECTION ( 'NONE',  ( 0.000000000000000000, 0.000000000000000000, -1.000000000000000000 ) ) ;
#9406 = CARTESIAN_POINT ( 'NONE',  ( -151.4692556286852891, -163.7391397928655010, 60.17163382399899518 ) ) ;
#9407 = VECTOR ( 'NONE', #9865, 1000.000000000000114 ) ;
#9408 = DIRECTION ( 'NONE',  ( -0.000000000000000000, 1.000000000000000000, -0.000000000000000000 ) ) ;
#9409 = LINE ( 'NONE', #14564, #11168 ) ;
#9410 = LINE ( 'NONE', #3905, #1118 ) ;
#9411 = VERTEX_POINT ( 'NONE', #6158 ) ;
#9412 = CARTESIAN_POINT ( 'NONE',  ( 47.43856463449117200, 80.02977050742732956, 32.77220824515698183 ) ) ;
#9413 = CARTESIAN_POINT ( 'NONE',  ( -151.4692556286852891, -161.6438272943107393, 39.74470866294723947 ) ) ;
#9414 = CARTESIAN_POINT ( 'NONE',  ( 10.61900875472251649, 108.8314319666055212, -5.279948415675857376 ) ) ;
#9415 = CARTESIAN_POINT ( 'NONE',  ( 43.01140435219951996, 10.71049967264875491, 39.21067981925356349 ) ) ;
#9416 = EDGE_LOOP ( 'NONE', ( #6460, #14119, #19521, #5774 ) ) ;
#9417 = FACE_OUTER_BOUND ( 'NONE', #13271, .T. ) ;
#9418 = CARTESIAN_POINT ( 'NONE',  ( 79.42064422693164261, 282.0082918409407284, 272.0939500981630204 ) ) ;
#9419 = CARTESIAN_POINT ( 'NONE',  ( 38.58424406990785371, 123.2297705074273040, 32.77220824515697473 ) ) ;
#9420 = CIRCLE ( 'NONE', #21741, 14.42424326798555434 ) ;
#9421 = ORIENTED_EDGE ( 'NONE', *, *, #15285, .T. ) ;
#9422 = DIRECTION ( 'NONE',  ( 1.000000000000000000, 0.000000000000000000, 0.000000000000000000 ) ) ;
#9423 = VERTEX_POINT ( 'NONE', #12894 ) ;
#9424 = CARTESIAN_POINT ( 'NONE',  ( 40.27526882409969033, 129.8297705074273267, 37.97664729208901946 ) ) ;
#9425 = AXIS2_PLACEMENT_3D ( 'NONE', #13165, #14917, #6331 ) ;
#9426 = FACE_OUTER_BOUND ( 'NONE', #2468, .T. ) ;
#9427 = CARTESIAN_POINT ( 'NONE',  ( 39.42975644700377558, 90.07977050742732672, 31.60846029578754468 ) ) ;
#9428 = CARTESIAN_POINT ( 'NONE',  ( 39.92123440845004723, 65.33445800887257349, 29.95742577749337343 ) ) ;
#9429 = EDGE_CURVE ( 'NONE', #2116, #19966, #1643, .T. ) ;
#9430 =( REPRESENTATION_RELATIONSHIP ('NONE','NONE', #6933, #8609 ) REPRESENTATION_RELATIONSHIP_WITH_TRANSFORMATION ( #18572 )SHAPE_REPRESENTATION_RELATIONSHIP( ) );
#9431 = DIRECTION ( 'NONE',  ( 0.000000000000000000, 0.000000000000000000, 1.000000000000000000 ) ) ;
#9432 = LINE ( 'NONE', #9541, #2195 ) ;
#9433 = CARTESIAN_POINT ( 'NONE',  ( 41.46631938032478359, 97.31049967264873146, 38.96596240072933170 ) ) ;
#9434 = CARTESIAN_POINT ( 'NONE',  ( -154.5594255724347761, -189.0891397928654953, 40.14644641866476604 ) ) ;
#9435 = AXIS2_PLACEMENT_3D ( 'NONE', #3720, #18815, #8578 ) ;
#9436 = CARTESIAN_POINT ( 'NONE',  ( 41.46631938032478359, 67.31049967264873146, 38.96596240072933170 ) ) ;
#9437 = CARTESIAN_POINT ( 'NONE',  ( 48.01140435219951996, 125.0604996726487599, 35.83527830041809636 ) ) ;
#9438 = CARTESIAN_POINT ( 'NONE',  ( -157.2955611005346270, -188.3438272943107279, 41.63779006702063867 ) ) ;
#9439 = APPLICATION_PROTOCOL_DEFINITION ( 'draft international standard', 'automotive_design', 1998, #10848 ) ;
#9440 = AXIS2_PLACEMENT_3D ( 'NONE', #1273, #6340, #19793 ) ;
#9441 = CARTESIAN_POINT ( 'NONE',  ( 48.01140435219951996, 136.4344580088725820, 32.58608133808903773 ) ) ;
#9442 = CARTESIAN_POINT ( 'NONE',  ( 39.42975644700377558, 102.0797705074273267, 31.60846029578754468 ) ) ;
#9443 = CARTESIAN_POINT ( 'NONE',  ( 38.01409278319488294, 147.7425775668531003, 9.723292677533123651 ) ) ;
#9444 = CARTESIAN_POINT ( 'NONE',  ( -157.2955611005346270, -191.3438272943106995, 41.63779006702063867 ) ) ;
#9445 = CARTESIAN_POINT ( 'NONE',  ( 47.43856463449117911, 100.7651871740939953, 32.77220824515697473 ) ) ;
#9446 = AXIS2_PLACEMENT_3D ( 'NONE', #9168, #15867, #20953 ) ;
#9447 = DIRECTION ( 'NONE',  ( 1.000000000000000000, 0.000000000000000000, 0.000000000000000000 ) ) ;
#9448 = EDGE_LOOP ( 'NONE', ( #5632, #2987, #7411, #8776 ) ) ;
#9449 = CARTESIAN_POINT ( 'NONE',  ( 43.01140435219951996, 158.9604996726487514, 29.21067981925357060 ) ) ;
#9450 = CARTESIAN_POINT ( 'NONE',  ( 76.66991938639012005, 113.6622739410785670, 5.791450954060403333 ) ) ;
#9451 = CARTESIAN_POINT ( 'NONE',  ( 15.80414578680225723, 112.4924633436790344, 15.87081086175909306 ) ) ;
#9452 = CARTESIAN_POINT ( 'NONE',  ( 46.10157429594899270, 154.7344580088725650, 29.95742577749336988 ) ) ;
#9453 = CARTESIAN_POINT ( 'NONE',  ( 38.58424406990786082, 69.37977050742730967, 34.21067981925357060 ) ) ;
#9454 = VERTEX_POINT ( 'NONE', #1102 ) ;
#9455 = ORIENTED_EDGE ( 'NONE', *, *, #1610, .T. ) ;
#9456 = CARTESIAN_POINT ( 'NONE',  ( 39.42975644700377558, 153.6797705074273210, 36.81289934271958941 ) ) ;
#9457 = CARTESIAN_POINT ( 'NONE',  ( 38.01140435219951996, 120.5604996726487457, 32.58608133808903773 ) ) ;
#9459 = CARTESIAN_POINT ( 'NONE',  ( 14.43535904578935103, 101.2031681353820574, 9.438814132600386486 ) ) ;
#9458 = CARTESIAN_POINT ( 'NONE',  ( 47.43856463449118621, 79.61518717409400381, 34.21067981925357060 ) ) ;
#9460 = CARTESIAN_POINT ( 'NONE',  ( 43.01140435219951996, 10.71049967264875491, 39.21067981925356349 ) ) ;
#9461 = EDGE_CURVE ( 'NONE', #8176, #21618, #14298, .T. ) ;
#9462 = CARTESIAN_POINT ( 'NONE',  ( -154.3824083646099439, -172.2938272943107165, 58.62277379824867296 ) ) ;
#9463 = CARTESIAN_POINT ( 'NONE',  ( 21.43032318156618388, 146.4805633285969861, 10.07716523980869816 ) ) ;
#9464 = CARTESIAN_POINT ( 'NONE',  ( -143.3790856849358306, -189.3630981290893089, 55.53486410454105027 ) ) ;
#9465 = DIRECTION ( 'NONE',  ( 0.000000000000000000, 1.000000000000000000, 0.000000000000000000 ) ) ;
#9467 = EDGE_CURVE ( 'NONE', #8778, #10077, #12458, .T. ) ;
#9466 = CARTESIAN_POINT ( 'NONE',  ( 38.96631938032478359, 150.0844580088725593, 37.14960608071593384 ) ) ;
#9468 = CARTESIAN_POINT ( 'NONE',  ( 45.74753988029933538, 131.3297705074273267, 30.44471234641811819 ) ) ;
#9469 = CARTESIAN_POINT ( 'NONE',  ( 61.24245875951225315, 90.83725678726602837, 5.715745788549559059 ) ) ;
#9470 = CARTESIAN_POINT ( 'NONE',  ( 47.43856463449118621, 130.6151871740940180, 34.21067981925357060 ) ) ;
#9471 = CARTESIAN_POINT ( 'NONE',  ( 39.92123440845005433, 69.26049967264874851, 29.95742577749336988 ) ) ;
#9472 = CARTESIAN_POINT ( 'NONE',  ( 41.46631938032478359, 150.1104996726487570, 29.45539723777780239 ) ) ;
#9473 = CARTESIAN_POINT ( 'NONE',  ( 43.80332655382220253, 64.53738109496899256, 39.21067981925355639 ) ) ;
#9474 = DIRECTION ( 'NONE',  ( -1.000000000000000000, 0.000000000000000000, 0.000000000000000000 ) ) ;
#9475 = CARTESIAN_POINT ( 'NONE',  ( 40.03295031927941494, 147.9482203214073479, -10.20071078494585670 ) ) ;
#9476 = DIRECTION ( 'NONE',  ( 0.000000000000000000, 1.000000000000000000, 0.000000000000000000 ) ) ;
#9477 = CARTESIAN_POINT ( 'NONE',  ( 45.74753988029933538, 107.0651871740939640, 30.44471234641811819 ) ) ;
#9478 = ORIENTED_EDGE ( 'NONE', *, *, #9514, .F. ) ;
#9479 = ADVANCED_FACE ( 'NONE', ( #17731 ), #19188, .F. ) ;
#9480 = CARTESIAN_POINT ( 'NONE',  ( -145.2889157411863437, -157.4391397928654612, 58.16351966513671812 ) ) ;
#9481 = ORIENTED_EDGE ( 'NONE', *, *, #8338, .F. ) ;
#9482 = CARTESIAN_POINT ( 'NONE',  ( 41.46631938032478359, 90.38445800887258486, 38.96596240072933170 ) ) ;
#9483 = CARTESIAN_POINT ( 'NONE',  ( 43.01140435219951996, 10.71049967264875491, 34.21067981925357060 ) ) ;
#9484 = CARTESIAN_POINT ( 'NONE',  ( 48.01140435219951996, 152.3604996726487570, 32.58608133808903773 ) ) ;
#9486 = CARTESIAN_POINT ( 'NONE',  ( 32.21091799184858218, 93.94358800413606048, -12.14875741943239085 ) ) ;
#9485 = CARTESIAN_POINT ( 'NONE',  ( 39.42975644700377558, 108.4151871740940152, 36.81289934271958941 ) ) ;
#9487 = EDGE_CURVE ( 'NONE', #12850, #9846, #12568, .T. ) ;
#9488 = CARTESIAN_POINT ( 'NONE',  ( 11.17254549292281318, -61.68114226949890622, -46.21320343559645494 ) ) ;
#9490 = CARTESIAN_POINT ( 'NONE',  ( -145.2889157411863437, -182.6130981290893374, 41.15050349809589392 ) ) ;
#9489 = CARTESIAN_POINT ( 'NONE',  ( 43.34257982665531728, 144.9070776186055696, 39.21067981925357060 ) ) ;
#9491 = AXIS2_PLACEMENT_3D ( 'NONE', #21270, #6149, #19604 ) ;
#9492 = FACE_OUTER_BOUND ( 'NONE', #1001, .T. ) ;
#9493 = DIRECTION ( 'NONE',  ( 1.723963091245776585E-16, 6.336983651701954299E-17, 1.000000000000000000 ) ) ;
#9494 = CARTESIAN_POINT ( 'NONE',  ( 41.64333658814960870, 62.51518717409400239, 30.00020018409699318 ) ) ;
#9495 = CARTESIAN_POINT ( 'NONE',  ( 77.22348061889915982, 118.7203125366680752, -8.375138532479306619 ) ) ;
#9496 = EDGE_CURVE ( 'NONE', #10959, #19332, #12783, .T. ) ;
#9497 = CARTESIAN_POINT ( 'NONE',  ( 47.05648932407426344, 95.51049967264873430, 31.27175355779120025 ) ) ;
#9498 = CARTESIAN_POINT ( 'NONE',  ( -142.0420953463935803, -174.5438272943107449, 52.72008163687743831 ) ) ;
#9499 = CARTESIAN_POINT ( 'NONE',  ( -142.0420953463935803, -189.5084106276440536, 46.59394152635518083 ) ) ;
#9500 = ORIENTED_EDGE ( 'NONE', *, *, #10121, .T. ) ;
#9501 = CARTESIAN_POINT ( 'NONE',  ( 44.37947211624943833, 68.21518717409399812, 30.00020018409699318 ) ) ;
#9502 = CARTESIAN_POINT ( 'NONE',  ( -157.2955611005346270, -173.6084106276440480, 41.63779006702063867 ) ) ;
#9503 = CARTESIAN_POINT ( 'NONE',  ( 75.94266982333172677, 110.2653427511449422, 11.90618179609112026 ) ) ;
#9504 = LINE ( 'NONE', #8172, #11980 ) ;
#9505 = CARTESIAN_POINT ( 'NONE',  ( 38.58424406990784661, 135.2651871740939953, 35.64915139335016647 ) ) ;
#9506 = VERTEX_POINT ( 'NONE', #17628 ) ;
#9507 = VERTEX_POINT ( 'NONE', #2536 ) ;
#9508 = EDGE_CURVE ( 'NONE', #5609, #20418, #884, .T. ) ;
#9509 = VECTOR ( 'NONE', #293, 1000.000000000000000 ) ;
#9510 = SURFACE_STYLE_USAGE ( .BOTH. , #2770 ) ;
#9511 = ORIENTED_EDGE ( 'NONE', *, *, #21604, .T. ) ;
#9512 = CARTESIAN_POINT ( 'NONE',  ( 47.05648932407426344, 117.9844580088725792, 37.14960608071593384 ) ) ;
#9513 = CARTESIAN_POINT ( 'NONE',  ( 44.55648932407425633, 59.81049967264874567, 29.45539723777780239 ) ) ;
#9514 = EDGE_CURVE ( 'NONE', #1555, #15249, #21640, .T. ) ;
#9515 = CARTESIAN_POINT ( 'NONE',  ( 45.74753988029933538, 77.32977050742729830, 30.44471234641811819 ) ) ;
#9516 = CARTESIAN_POINT ( 'NONE',  ( 46.59305225739526435, 136.3151871740940351, 36.81289934271958941 ) ) ;
#9517 = CARTESIAN_POINT ( 'NONE',  ( 38.01140435219951996, 87.56049967264871725, 32.58608133808903773 ) ) ;
#9518 = CARTESIAN_POINT ( 'NONE',  ( 35.69068542950036260, 86.46542255174357194, 7.577194441455407770 ) ) ;
#9519 = CARTESIAN_POINT ( 'NONE',  ( 38.52064617801426749, 95.31338828682366682, 31.98784611697848135 ) ) ;
#9520 = CARTESIAN_POINT ( 'NONE',  ( -151.4692556286852891, -160.7391397928654726, 60.17163382399899518 ) ) ;
#9521 = CARTESIAN_POINT ( 'NONE',  ( 43.80332655382220253, 106.5373810949690068, 39.21067981925355639 ) ) ;
#9522 = CARTESIAN_POINT ( 'NONE',  ( 48.01140435219951996, 62.36049967264873573, 32.58608133808903773 ) ) ;
#9523 =( GEOMETRIC_REPRESENTATION_CONTEXT ( 3 ) GLOBAL_UNCERTAINTY_ASSIGNED_CONTEXT ( ( #8438 ) ) GLOBAL_UNIT_ASSIGNED_CONTEXT ( ( #21622, #11138, #21293 ) ) REPRESENTATION_CONTEXT ( 'NONE', 'WORKASPACE' ) );
#9524 = ORIENTED_EDGE ( 'NONE', *, *, #20404, .T. ) ;
#9525 = CARTESIAN_POINT ( 'NONE',  ( 43.01140435219951286, 71.62977050742732388, 29.55568802177586463 ) ) ;
#9526 = EDGE_CURVE ( 'NONE', #20108, #4552, #9816, .T. ) ;
#9527 = CARTESIAN_POINT ( 'NONE',  ( -160.8964159109769696, -194.0084106276440252, 52.72008163687743121 ) ) ;
#9528 = CARTESIAN_POINT ( 'NONE',  ( 36.38086904327614235, 86.32171732562966326, 0.5532606071062302622 ) ) ;
#9529 = CARTESIAN_POINT ( 'NONE',  ( -154.3824083646099439, -188.7584106276440536, 40.69124936498395328 ) ) ;
#9530 = VERTEX_POINT ( 'NONE', #14972 ) ;
#9531 = CYLINDRICAL_SURFACE ( 'NONE', #12892, 10.00000000000000888 ) ;
#9532 = DIRECTION ( 'NONE',  ( -0.000000000000000000, -0.000000000000000000, -1.000000000000000000 ) ) ;
#9533 = CARTESIAN_POINT ( 'NONE',  ( 41.64333658814960870, 125.7797705074273296, 30.00020018409699318 ) ) ;
#9534 = ORIENTED_EDGE ( 'NONE', *, *, #21084, .T. ) ;
#9535 = DIRECTION ( 'NONE',  ( -0.000000000000000000, -0.000000000000000000, -1.000000000000000000 ) ) ;
#9536 =( BOUNDED_CURVE ( )  B_SPLINE_CURVE ( 2, ( #3017, #13050, #9755, #6097, #1147 ),
 .UNSPECIFIED., .F., .T. ) 
 B_SPLINE_CURVE_WITH_KNOTS ( ( 3, 2, 3 ),
 ( 0.9779411764705882026, 0.9794117647058823151, 0.9803957504473121976 ),
 .UNSPECIFIED. ) 
 CURVE ( )  GEOMETRIC_REPRESENTATION_ITEM ( )  RATIONAL_B_SPLINE_CURVE ( ( 0.9755282581475768211, 0.9755282581475768211, 1.000000000000000000, 0.9836257053654985372, 0.9782076199944956807 ) ) 
 REPRESENTATION_ITEM ( '' )  );
#9537 = ORIENTED_EDGE ( 'NONE', *, *, #13099, .T. ) ;
#9538 = CARTESIAN_POINT ( 'NONE',  ( 45.74753988029933538, 131.3297705074273267, 30.44471234641811819 ) ) ;
#9539 = CARTESIAN_POINT ( 'NONE',  ( 44.55648932407425633, 58.88445800887258486, 29.45539723777780239 ) ) ;
#9540 = FACE_OUTER_BOUND ( 'NONE', #6548, .T. ) ;
#9541 = CARTESIAN_POINT ( 'NONE',  ( -138.5468111011521160, 759.4679229819337252, -23.16745088979876499 ) ) ;
#9542 = CARTESIAN_POINT ( 'NONE',  ( -157.6495955161842062, -185.0391397928653987, 58.16351966513671812 ) ) ;
#9543 = DIRECTION ( 'NONE',  ( 0.000000000000000000, 1.000000000000000000, 0.000000000000000000 ) ) ;
#9544 = DIRECTION ( 'NONE',  ( -0.000000000000000000, -0.000000000000000000, -1.000000000000000000 ) ) ;
#9545 = CARTESIAN_POINT ( 'NONE',  ( -142.0420953463935803, -192.2438272943107336, 46.59394152635518793 ) ) ;
#9546 = APPLICATION_PROTOCOL_DEFINITION ( 'draft international standard', 'automotive_design', 1998, #4779 ) ;
#9547 = CARTESIAN_POINT ( 'NONE',  ( 39.92123440845004723, 122.3344580088725593, 29.95742577749337343 ) ) ;
#9548 = CARTESIAN_POINT ( 'NONE',  ( 44.37947211624943833, 100.2797705074273154, 38.42115945441014446 ) ) ;
#9549 = CARTESIAN_POINT ( 'NONE',  ( 15.53544334784188585, 126.6048195653137469, 15.43757839183889224 ) ) ;
#9550 = CARTESIAN_POINT ( 'NONE',  ( -159.0959885057557983, -187.5938272943107279, 55.19815736654470584 ) ) ;
#9551 = CARTESIAN_POINT ( 'NONE',  ( 39.42975644700377558, 101.8151871740940067, 31.60846029578754468 ) ) ;
#9552 = CARTESIAN_POINT ( 'NONE',  ( 163.1026836591718734, 192.4288937294299160, 34.00000000000001421 ) ) ;
#9553 = VERTEX_POINT ( 'NONE', #13220 ) ;
#9554 = CARTESIAN_POINT ( 'NONE',  ( -151.4692556286852891, -177.2391397928654442, 39.65701158161629536 ) ) ;
#9555 = CARTESIAN_POINT ( 'NONE',  ( 20.88913110926514705, 146.0313881486468119, 3.053432864643822686 ) ) ;
#9556 = CARTESIAN_POINT ( 'NONE',  ( 26.87902611899987448, 142.9395564687116007, -9.767670631928341507 ) ) ;
#9557 = CARTESIAN_POINT ( 'NONE',  ( 43.01140435219951286, 71.62977050742732388, 29.55568802177586107 ) ) ;
#9558 = ORIENTED_EDGE ( 'NONE', *, *, #2230, .T. ) ;
#9559 = ORIENTED_EDGE ( 'NONE', *, *, #14093, .T. ) ;
#9560 = CARTESIAN_POINT ( 'NONE',  ( 39.42975644700377558, 150.6797705074273210, 36.81289934271958941 ) ) ;
#9561 = CARTESIAN_POINT ( 'NONE',  ( -161.4692556286852891, -193.4130981290892919, 52.90620854394536821 ) ) ;
#9562 = EDGE_CURVE ( 'NONE', #3562, #10959, #6575, .T. ) ;
#9563 = CARTESIAN_POINT ( 'NONE',  ( 48.01140435219951996, 110.2104996726487514, 34.21067981925357060 ) ) ;
#9565 = CARTESIAN_POINT ( 'NONE',  ( 68.08897506277223499, 96.72110655255949041, 7.414802352519190620 ) ) ;
#9564 = CARTESIAN_POINT ( 'NONE',  ( 46.59305225739526435, 64.91518717409400097, 31.60846029578754468 ) ) ;
#9566 = CARTESIAN_POINT ( 'NONE',  ( 39.92123440845005433, 96.23445800887257917, 38.46393386101375711 ) ) ;
#9567 = CARTESIAN_POINT ( 'NONE',  ( -143.8425227516148084, -171.0938272943107279, 44.11586579668791330 ) ) ;
#9568 = CARTESIAN_POINT ( 'NONE',  ( 163.1026836591718734, 192.4288937294299160, 18.98992973508700643 ) ) ;
#9569 = CARTESIAN_POINT ( 'NONE',  ( -143.3790856849358306, -177.3630981290893089, 55.53486410454105027 ) ) ;
#9570 = LINE ( 'NONE', #7916, #20571 ) ;
#9571 = CARTESIAN_POINT ( 'NONE',  ( 38.01140435219951996, 149.6344580088725991, 32.58608133808903773 ) ) ;
#9572 = CARTESIAN_POINT ( 'NONE',  ( 43.01140435219951286, 128.6297705074273097, 29.55568802177586463 ) ) ;
#9573 = CARTESIAN_POINT ( 'NONE',  ( 22.95395889711706872, 147.7494453258605915, 2.144227187454380790 ) ) ;
#9574 = CARTESIAN_POINT ( 'NONE',  ( 39.42975644700377558, 123.4151871740940010, 36.81289934271958941 ) ) ;
#9575 =( LENGTH_UNIT ( ) NAMED_UNIT ( * ) SI_UNIT ( .MILLI., .METRE. ) );
#9576 = AXIS2_PLACEMENT_3D ( 'NONE', #7084, #18546, #3336 ) ;
#9577 = CARTESIAN_POINT ( 'NONE',  ( -143.8425227516148084, -156.3584106276440480, 44.11586579668791330 ) ) ;
#9579 = CARTESIAN_POINT ( 'NONE',  ( 48.01140435219951996, 65.36049967264874283, 32.58608133808903773 ) ) ;
#9578 = VECTOR ( 'NONE', #7169, 1000.000000000000227 ) ;
#9580 = CARTESIAN_POINT ( 'NONE',  ( 173.3794444120442506, -126.9891397928655010, 67.64809332337412684 ) ) ;
#9581 = CARTESIAN_POINT ( 'NONE',  ( 69.69253243162556544, 129.2828754355126648, 18.29472124897268159 ) ) ;
#9582 = DIRECTION ( 'NONE',  ( 0.000000000000000000, 0.000000000000000000, -1.000000000000000000 ) ) ;
#9583 = AXIS2_PLACEMENT_3D ( 'NONE', #5789, #1053, #17472 ) ;
#9584 = ORIENTED_EDGE ( 'NONE', *, *, #1011, .T. ) ;
#9585 = CARTESIAN_POINT ( 'NONE',  ( 46.10157429594899270, 85.76049967264874851, 38.46393386101375711 ) ) ;
#9586 = ORIENTED_EDGE ( 'NONE', *, *, #18437, .T. ) ;
#9587 = CARTESIAN_POINT ( 'NONE',  ( 38.96631938032478359, 86.48445800887257917, 31.27175355779120025 ) ) ;
#9588 = CARTESIAN_POINT ( 'NONE',  ( 147.5268905834513475, 193.0332408774651185, -29.99999999999997868 ) ) ;
#9589 = AXIS2_PLACEMENT_3D ( 'NONE', #20294, #8510, #9943 ) ;
#9590 = AXIS2_PLACEMENT_3D ( 'NONE', #16063, #7714, #14415 ) ;
#9591 = CARTESIAN_POINT ( 'NONE',  ( 46.10157429594899270, 145.7604996726487627, 38.46393386101376421 ) ) ;
#9593 = CARTESIAN_POINT ( 'NONE',  ( 61.95829188091916961, 99.12855633088805973, 0.5892133286805102399 ) ) ;
#9592 = CARTESIAN_POINT ( 'NONE',  ( 39.42975644700377558, 93.41518717409400097, 36.81289934271958941 ) ) ;
#9594 = CARTESIAN_POINT ( 'NONE',  ( -159.0959885057557983, -170.4584106276440423, 44.11586579668791330 ) ) ;
#9595 = CARTESIAN_POINT ( 'NONE',  ( 39.92123440845004723, 64.16049967264873999, 38.46393386101376421 ) ) ;
#9597 = CARTESIAN_POINT ( 'NONE',  ( 43.01140435219951996, 170.7104996726487514, 34.21067981925357060 ) ) ;
#9596 = CARTESIAN_POINT ( 'NONE',  ( 72.34521997529867576, 314.8592298662555322, 4.000000000000003553 ) ) ;
#9598 = CARTESIAN_POINT ( 'NONE',  ( -149.8854112254399240, -188.3899795514095956, 39.65701158161630957 ) ) ;
#9599 = DIRECTION ( 'NONE',  ( -0.000000000000000000, -0.000000000000000000, -1.000000000000000000 ) ) ;
#9600 = CARTESIAN_POINT ( 'NONE',  ( -151.4692556286852891, -196.9891397928655010, 59.65701158161632378 ) ) ;
#9601 = CARTESIAN_POINT ( 'NONE',  ( 47.43856463449117200, 157.7297705074273040, 35.64915139335016647 ) ) ;
#9602 = CARTESIAN_POINT ( 'NONE',  ( 15.39564893635072806, 140.1373336744895255, -4.208549045858890558 ) ) ;
#9603 = CARTESIAN_POINT ( 'NONE',  ( 41.64333658814960870, 150.7151871740940123, 38.42115945441014446 ) ) ;
#9604 = CARTESIAN_POINT ( 'NONE',  ( 57.67197451322198276, 240.2871645992281628, -45.62971374797768220 ) ) ;
#9605 = CARTESIAN_POINT ( 'NONE',  ( -160.8964159109769696, -173.0438272943107449, 46.59394152635518793 ) ) ;
#9606 = CARTESIAN_POINT ( 'NONE',  ( -145.6429501568359797, -180.2084106276440707, 41.63779006702063867 ) ) ;
#9607 = EDGE_LOOP ( 'NONE', ( #14010, #10159, #17768, #19089 ) ) ;
#9608 = CARTESIAN_POINT ( 'NONE',  ( 45.74753988029934249, 65.06518717409400665, 30.44471234641812174 ) ) ;
#9609 = EDGE_CURVE ( 'NONE', #4967, #119, #4843, .T. ) ;
#9610 = CARTESIAN_POINT ( 'NONE',  ( -157.2955611005346270, -166.7084106276440423, 57.67623309621198047 ) ) ;
#9611 = CARTESIAN_POINT ( 'NONE',  ( 30.67228459367742133, 151.9265198579663263, 16.42994147312239051 ) ) ;
#9612 = FACE_OUTER_BOUND ( 'NONE', #10750, .T. ) ;
#9613 = CARTESIAN_POINT ( 'NONE',  ( 47.43856463449118621, 130.6151871740940180, 34.21067981925357060 ) ) ;
#9614 = CARTESIAN_POINT ( 'NONE',  ( 73.15003751907750029, 103.8404476760371864, -6.870911935119222491 ) ) ;
#9615 = EDGE_LOOP ( 'NONE', ( #17671, #15270, #13021, #4496 ) ) ;
#9616 = ORIENTED_EDGE ( 'NONE', *, *, #11847, .F. ) ;
#9617 =( NAMED_UNIT ( * ) SI_UNIT ( $, .STERADIAN. ) SOLID_ANGLE_UNIT ( ) );
#9618 = ORIENTED_EDGE ( 'NONE', *, *, #20429, .T. ) ;
#9619 = CARTESIAN_POINT ( 'NONE',  ( 43.01140435219951286, 116.9604996726487371, 29.21067981925356705 ) ) ;
#9620 = CARTESIAN_POINT ( 'NONE',  ( 39.42975644700377558, 75.67977050742732104, 36.81289934271958941 ) ) ;
#9622 = CARTESIAN_POINT ( 'NONE',  ( 15.53003795322992353, 126.2325256570730687, 2.418278830334454899 ) ) ;
#9621 = CARTESIAN_POINT ( 'NONE',  ( 38.58424406990784661, 137.9651871740939839, 32.77220824515698183 ) ) ;
#9623 = CARTESIAN_POINT ( 'NONE',  ( 44.55648932407425633, 94.61049967264874283, 38.96596240072933170 ) ) ;
#9624 = CARTESIAN_POINT ( 'NONE',  ( 30.90322180743143576, 151.9278386122780375, 10.43433729856376502 ) ) ;
#9625 = CARTESIAN_POINT ( 'NONE',  ( 38.26843650118725293, 95.36078014034055172, 32.59446367923827381 ) ) ;
#9626 = CARTESIAN_POINT ( 'NONE',  ( -154.5594255724347761, -160.8891397928654499, 59.16757674456785310 ) ) ;
#9627 = CARTESIAN_POINT ( 'NONE',  ( 43.01140435219951286, 83.36518717409397539, 29.55568802177586463 ) ) ;
#9628 = CARTESIAN_POINT ( 'NONE',  ( 42.68014329765944126, 144.9070776186055696, 39.21067981925356349 ) ) ;
#9629 = DIRECTION ( 'NONE',  ( -0.000000000000000000, 1.000000000000000000, -0.000000000000000000 ) ) ;
#9630 = DIRECTION ( 'NONE',  ( 0.000000000000000000, 1.000000000000000000, 0.000000000000000000 ) ) ;
#9631 = ORIENTED_EDGE ( 'NONE', *, *, #5582, .T. ) ;
#9632 = CARTESIAN_POINT ( 'NONE',  ( 39.42975644700377558, 78.07977050742731251, 31.60846029578754468 ) ) ;
#9633 = CARTESIAN_POINT ( 'NONE',  ( -142.0420953463935803, -192.8084106276440650, 52.72008163687743831 ) ) ;
#9634 = CARTESIAN_POINT ( 'NONE',  ( 9.822352152143091431, 128.2981216602131553, 9.363167623699879982 ) ) ;
#9635 = CARTESIAN_POINT ( 'NONE',  ( -148.5561028927606344, -183.0584106276440650, 40.69124936498395328 ) ) ;
#9636 = ORIENTED_EDGE ( 'NONE', *, *, #19879, .F. ) ;
#9637 = CARTESIAN_POINT ( 'NONE',  ( 38.58424406990786082, 159.1151871740940180, 34.21067981925357060 ) ) ;
#9638 = DIRECTION ( 'NONE',  ( 0.000000000000000000, 0.000000000000000000, 1.000000000000000000 ) ) ;
#9639 = EDGE_CURVE ( 'NONE', #6227, #6453, #6387, .T. ) ;
#9640 = CARTESIAN_POINT ( 'NONE',  ( 44.37947211624943833, 122.4797705074273182, 30.00020018409699318 ) ) ;
#9641 = ORIENTED_EDGE ( 'NONE', *, *, #18588, .F. ) ;
#9642 = ORIENTED_EDGE ( 'NONE', *, *, #333, .T. ) ;
#9643 = CARTESIAN_POINT ( 'NONE',  ( 47.43856463449117200, 124.7297705074273182, 35.64915139335016647 ) ) ;
#9644 = CARTESIAN_POINT ( 'NONE',  ( 38.96631938032478359, 73.01049967264873430, 37.14960608071593384 ) ) ;
#9645 = CARTESIAN_POINT ( 'NONE',  ( 46.59305225739526435, 89.17977050742732104, 31.60846029578754468 ) ) ;
#9646 = CARTESIAN_POINT ( 'NONE',  ( 43.01140435219951286, 63.53445800887257633, 39.46799094044489209 ) ) ;
#9647 = DIRECTION ( 'NONE',  ( -1.000000000000000000, 0.000000000000000000, 0.000000000000000000 ) ) ;
#9648 = CARTESIAN_POINT ( 'NONE',  ( 43.01140435219951996, 10.71049967264875491, 34.21067981925357060 ) ) ;
#9649 = CARTESIAN_POINT ( 'NONE',  ( 39.92123440845005433, 97.16049967264873999, 38.46393386101375711 ) ) ;
#9650 = CARTESIAN_POINT ( 'NONE',  ( -148.3790856849358306, -192.3891397928654783, 40.14644641866477315 ) ) ;
#9651 = CARTESIAN_POINT ( 'NONE',  ( 147.8787791192428074, -136.9891397928655010, 49.65701158161629536 ) ) ;
#9652 = CARTESIAN_POINT ( 'NONE',  ( 42.21948215057684450, 103.3836182503284675, 39.21067981925355639 ) ) ;
#9653 = CARTESIAN_POINT ( 'NONE',  ( -143.8425227516148084, -189.0938272943107279, 44.11586579668791330 ) ) ;
#9654 = PRODUCT_CONTEXT ( 'NONE', #21405, 'mechanical' ) ;
#9655 = EDGE_CURVE ( 'NONE', #18126, #3562, #3488, .T. ) ;
#9656 = CARTESIAN_POINT ( 'NONE',  ( 47.05648932407426344, 120.9844580088725934, 37.14960608071593384 ) ) ;
#9657 = CARTESIAN_POINT ( 'NONE',  ( 38.58424406990786082, 108.3797705074273239, 34.21067981925357060 ) ) ;
#9658 = CARTESIAN_POINT ( 'NONE',  ( 44.65913741311992879, 148.1402468479653578, 16.98531508000710843 ) ) ;
#9659 = CARTESIAN_POINT ( 'NONE',  ( -148.5561028927606344, -180.9938272943107336, 58.62277379824867296 ) ) ;
#9660 = CARTESIAN_POINT ( 'NONE',  ( 40.27526882409969744, 86.66518717409400097, 30.44471234641812174 ) ) ;
#9661 = FACE_OUTER_BOUND ( 'NONE', #11346, .T. ) ;
#9662 = ORIENTED_EDGE ( 'NONE', *, *, #5177, .T. ) ;
#9663 = CARTESIAN_POINT ( 'NONE',  ( 43.01140435219951996, 70.71049967264875136, 34.21067981925357060 ) ) ;
#9664 = CARTESIAN_POINT ( 'NONE',  ( 48.17517050666977241, 153.7480039124125994, 4.005852979123367241 ) ) ;
#9665 =( BOUNDED_CURVE ( )  B_SPLINE_CURVE ( 2, ( #16969, #224, #1777, #3437, #1880, #8179, #16532, #8613, #3322, #8398, #13668, #10051, #6961 ),
 .UNSPECIFIED., .F., .F. ) 
 B_SPLINE_CURVE_WITH_KNOTS ( ( 3, 2, 2, 2, 2, 2, 3 ),
 ( 0.4338235294117647189, 0.4352941176470588314, 0.4382352941176470562, 0.4411764705882352811, 0.4441176470588235059, 0.4470588235294117863, 0.4485294117647058987 ),
 .UNSPECIFIED. ) 
 CURVE ( )  GEOMETRIC_REPRESENTATION_ITEM ( )  RATIONAL_B_SPLINE_CURVE ( ( 0.9755282581475768211, 0.9755282581475768211, 1.000000000000000000, 0.9510565162951535312, 1.000000000000000000, 0.9510565162951535312, 1.000000000000000000, 0.9510565162951535312, 1.000000000000000000, 0.9510565162951535312, 1.000000000000000000, 0.9755282581475768211, 0.9755282581475768211 ) ) 
 REPRESENTATION_ITEM ( '' )  );
#9666 = CARTESIAN_POINT ( 'NONE',  ( 66.60919851020621252, 104.6140855887898624, -13.69650096386476079 ) ) ;
#9667 = CARTESIAN_POINT ( 'NONE',  ( 40.27526882409969744, 63.82977050742731961, 37.97664729208901235 ) ) ;
#9668 = ORIENTED_EDGE ( 'NONE', *, *, #8887, .F. ) ;
#9669 = ORIENTED_EDGE ( 'NONE', *, *, #14698, .F. ) ;
#9670 = CARTESIAN_POINT ( 'NONE',  ( 39.42975644700377558, 153.0797705074273267, 31.60846029578754468 ) ) ;
#9671 = LINE ( 'NONE', #6018, #10541 ) ;
#9672 = AXIS2_PLACEMENT_3D ( 'NONE', #19503, #9599, #19396 ) ;
#9673 = CARTESIAN_POINT ( 'NONE',  ( 48.01140435219951996, 113.2104996726487371, 34.21067981925357060 ) ) ;
#9674 = CARTESIAN_POINT ( 'NONE',  ( 41.64333658814960870, 69.71518717409399812, 38.42115945441014446 ) ) ;
#9675 = CARTESIAN_POINT ( 'NONE',  ( -151.4692556286852891, -155.9084106276440593, 39.74470866294723947 ) ) ;
#9676 = VECTOR ( 'NONE', #7159, 1000.000000000000000 ) ;
#9677 = CARTESIAN_POINT ( 'NONE',  ( -151.4692556286852891, -163.1438272943106824, 59.56931450028537256 ) ) ;
#9678 = CARTESIAN_POINT ( 'NONE',  ( -151.4692556286853176, -165.2391397928654442, 39.65701158161629536 ) ) ;
#9679 = CARTESIAN_POINT ( 'NONE',  ( -161.4692556286852607, -175.4130981290893203, 52.90620854394536821 ) ) ;
#9680 = SHAPE_REPRESENTATION_RELATIONSHIP ( 'NONE' , 'NONE' ,  #13805, #13742 ) ;
#9681 = EDGE_CURVE ( 'NONE', #9281, #14883, #11906, .T. ) ;
#9682 = CARTESIAN_POINT ( 'NONE',  ( -151.4692556286852607, -184.7391397928654726, 59.65701158161632378 ) ) ;
#9683 = CARTESIAN_POINT ( 'NONE',  ( 39.92123440845004723, 155.3344580088725877, 29.95742577749337343 ) ) ;
#9684 = CARTESIAN_POINT ( 'NONE',  ( 45.74753988029933538, 130.4297705074273210, 37.97664729208901946 ) ) ;
#9685 = CARTESIAN_POINT ( 'NONE',  ( 20.67200536010596323, 145.9528555770810385, 9.049038938933962939 ) ) ;
#9686 = CARTESIAN_POINT ( 'NONE',  ( 40.27526882409969744, 126.5651871740940067, 37.97664729208901235 ) ) ;
#9687 = CARTESIAN_POINT ( 'NONE',  ( 151.4773229304660731, 84.89323405393692212, 4.000000000000021316 ) ) ;
#9688 = CARTESIAN_POINT ( 'NONE',  ( -148.5561028927606344, -157.2584106276440536, 58.62277379824867296 ) ) ;
#9689 = CARTESIAN_POINT ( 'NONE',  ( 43.01140435219951996, 10.71049967264875491, 29.21067981925357060 ) ) ;
#9690 = CARTESIAN_POINT ( 'NONE',  ( 47.05648932407426344, 148.9104996726487400, 37.14960608071593384 ) ) ;
#9691 = CARTESIAN_POINT ( 'NONE',  ( 39.55749537675153960, 91.83829536962669238, 20.55682687220188143 ) ) ;
#9692 = DIRECTION ( 'NONE',  ( 0.000000000000000000, 1.000000000000000000, 0.000000000000000000 ) ) ;
#9693 = VERTEX_POINT ( 'NONE', #4960 ) ;
#9694 = DIRECTION ( 'NONE',  ( 0.000000000000000000, 0.000000000000000000, 1.000000000000000000 ) ) ;
#9695 = EDGE_LOOP ( 'NONE', ( #12135, #1657, #8067, #2793 ) ) ;
#9696 = CARTESIAN_POINT ( 'NONE',  ( 47.05648932407426344, 78.98445800887257917, 37.14960608071593384 ) ) ;
#9697 = CARTESIAN_POINT ( 'NONE',  ( 161.4773229304660731, 84.89323405393692212, 14.00000000000001776 ) ) ;
#9698 = CARTESIAN_POINT ( 'NONE',  ( 38.96631938032478359, 141.4104996726487400, 31.27175355779120025 ) ) ;
#9700 = CARTESIAN_POINT ( 'NONE',  ( 33.35040633798650589, 93.49848361726675705, 8.803757759246650494 ) ) ;
#9699 = CARTESIAN_POINT ( 'NONE',  ( 40.27526882409969033, 93.56518717409397823, 37.97664729208901946 ) ) ;
#9701 = DIRECTION ( 'NONE',  ( 0.000000000000000000, -1.000000000000000000, 0.000000000000000000 ) ) ;
#9702 = CARTESIAN_POINT ( 'NONE',  ( -160.8964159109769696, -167.1584106276440593, 49.65701158161630957 ) ) ;
#9703 = CARTESIAN_POINT ( 'NONE',  ( -157.2955611005345986, -188.3438272943107279, 41.63779006702063867 ) ) ;
#9705 = LINE ( 'NONE', #14755, #1630 ) ;
#9704 = CARTESIAN_POINT ( 'NONE',  ( 134.6380592378700101, 268.5785371414991687, -3.999999999999996447 ) ) ;
#9706 = CARTESIAN_POINT ( 'NONE',  ( 38.01140435219952707, 105.7104996726487371, 34.21067981925357060 ) ) ;
#9707 = CARTESIAN_POINT ( 'NONE',  ( -145.2889157411863437, -174.5391397928654840, 41.15050349809589392 ) ) ;
#9708 = CARTESIAN_POINT ( 'NONE',  ( 46.10157429594899270, 80.66049967264873999, 29.95742577749336988 ) ) ;
#9709 = CARTESIAN_POINT ( 'NONE',  ( 39.42975644700377558, 63.41518717409400097, 36.81289934271958941 ) ) ;
#9710 = CARTESIAN_POINT ( 'NONE',  ( 36.38086904327614235, 86.32171732562966326, 0.5532606071062302622 ) ) ;
#9711 = AXIS2_PLACEMENT_3D ( 'NONE', #9597, #4190, #2533 ) ;
#9712 = CARTESIAN_POINT ( 'NONE',  ( -154.3824083646099439, -160.2938272943107449, 58.62277379824867296 ) ) ;
#9713 = CARTESIAN_POINT ( 'NONE',  ( -160.8964159109769696, -185.1584106276440309, 49.65701158161630957 ) ) ;
#9714 = ORIENTED_EDGE ( 'NONE', *, *, #19995, .F. ) ;
#9715 = CARTESIAN_POINT ( 'NONE',  ( 40.27526882409969744, 71.66518717409400097, 30.44471234641812174 ) ) ;
#9716 = CARTESIAN_POINT ( 'NONE',  ( -143.8425227516148084, -168.9584106276440423, 55.19815736654470584 ) ) ;
#9717 = CARTESIAN_POINT ( 'NONE',  ( 75.17075062522994244, 131.8760474256973509, 11.19198414525841301 ) ) ;
#9718 = DIRECTION ( 'NONE',  ( -0.4999999999999993894, 0.000000000000000000, 0.8660254037844389297 ) ) ;
#9719 = CARTESIAN_POINT ( 'NONE',  ( 47.43856463449117200, 133.7651871740939669, 32.77220824515698183 ) ) ;
#9720 = CARTESIAN_POINT ( 'NONE',  ( 54.88857506304572809, 87.88569651147935247, -13.06129575545291210 ) ) ;
#9721 = ORIENTED_EDGE ( 'NONE', *, *, #13644, .F. ) ;
#9722 = VERTEX_POINT ( 'NONE', #3081 ) ;
#9723 =( REPRESENTATION_RELATIONSHIP ('NONE','NONE', #6933, #21416 ) REPRESENTATION_RELATIONSHIP_WITH_TRANSFORMATION ( #20231 )SHAPE_REPRESENTATION_RELATIONSHIP( ) );
#9724 = CIRCLE ( 'NONE', #206, 10.00000000000000888 ) ;
#9725 = CARTESIAN_POINT ( 'NONE',  ( 59.36841858216658352, 96.93634223693318575, 13.72768157422830981 ) ) ;
#9726 = AXIS2_PLACEMENT_3D ( 'NONE', #16803, #168, #13607 ) ;
#9727 = VERTEX_POINT ( 'NONE', #16514 ) ;
#9728 = CARTESIAN_POINT ( 'NONE',  ( 39.92123440845004723, 111.2344580088725507, 38.46393386101376421 ) ) ;
#9729 = CARTESIAN_POINT ( 'NONE',  ( 48.01140435219951996, 116.2104996726487371, 34.21067981925357060 ) ) ;
#9730 = CARTESIAN_POINT ( 'NONE',  ( 38.58424406990784661, 66.52977050742730114, 35.64915139335016647 ) ) ;
#9732 = CARTESIAN_POINT ( 'NONE',  ( 29.12819380265916180, 95.36133955912156068, 0.9897074016940036190 ) ) ;
#9731 = CARTESIAN_POINT ( 'NONE',  ( 40.27526882409969033, 122.6651871740939725, 30.44471234641811819 ) ) ;
#9733 = CARTESIAN_POINT ( 'NONE',  ( 47.05648932407426344, 91.91049967264873999, 37.14960608071593384 ) ) ;
#9734 = CARTESIAN_POINT ( 'NONE',  ( 148.6725454929228079, -61.68114226949890622, -46.21320343559645494 ) ) ;
#9735 = CARTESIAN_POINT ( 'NONE',  ( 38.01157040740503845, 95.41214629490136190, 33.87806037135995751 ) ) ;
#9736 = CARTESIAN_POINT ( 'NONE',  ( 38.01140435219952707, 138.5604996726487457, 32.58608133808903773 ) ) ;
#9737 = CARTESIAN_POINT ( 'NONE',  ( 46.59305225739526435, 91.91518717409400097, 31.60846029578754468 ) ) ;
#9738 = DIRECTION ( 'NONE',  ( -0.9393725726208707050, -0.3428981916074317349, 0.000000000000000000 ) ) ;
#9739 = DIRECTION ( 'NONE',  ( -0.000000000000000000, 1.000000000000000000, -0.000000000000000000 ) ) ;
#9740 = EDGE_CURVE ( 'NONE', #10077, #2927, #1431, .T. ) ;
#9741 = ORIENTED_EDGE ( 'NONE', *, *, #19082, .F. ) ;
#9742 = CARTESIAN_POINT ( 'NONE',  ( 41.64333658814960870, 78.97977050742731819, 38.42115945441014446 ) ) ;
#9743 = CARTESIAN_POINT ( 'NONE',  ( -157.2955611005346270, -157.4438272943107506, 57.67623309621198047 ) ) ;
#9744 = CARTESIAN_POINT ( 'NONE',  ( 61.76154402333882132, 148.5480768402654803, 4.482004293238171400 ) ) ;
#9745 = CARTESIAN_POINT ( 'NONE',  ( -159.0959885057557983, -184.8584106276440480, 55.19815736654470584 ) ) ;
#9746 = VERTEX_POINT ( 'NONE', #19055 ) ;
#9747 = CARTESIAN_POINT ( 'NONE',  ( -154.5594255724347761, -162.0891397928654669, 40.14644641866476604 ) ) ;
#9748 = VECTOR ( 'NONE', #12615, 1000.000000000000227 ) ;
#9749 = CARTESIAN_POINT ( 'NONE',  ( 141.1725454929228079, -61.68114226949890622, 20.00000000000001776 ) ) ;
#9750 = CARTESIAN_POINT ( 'NONE',  ( 40.27526882409969744, 123.8297705074273125, 37.97664729208901235 ) ) ;
#9751 = VERTEX_POINT ( 'NONE', #13865 ) ;
#9752 = CARTESIAN_POINT ( 'NONE',  ( -151.4692556286852891, -196.9891397928655010, 39.65701158161630246 ) ) ;
#9753 = VERTEX_POINT ( 'NONE', #531 ) ;
#9754 = CARTESIAN_POINT ( 'NONE',  ( 41.64333658814960870, 120.9797705074273182, 38.42115945441014446 ) ) ;
#9755 = CARTESIAN_POINT ( 'NONE',  ( 44.55648932407425633, 58.88445800887258486, 29.45539723777780239 ) ) ;
#9756 = EDGE_CURVE ( 'NONE', #18667, #20725, #5486, .T. ) ;
#9757 = CARTESIAN_POINT ( 'NONE',  ( 39.42975644700377558, 152.8151871740940067, 31.60846029578754468 ) ) ;
#9758 = CARTESIAN_POINT ( 'NONE',  ( -39.63192160874127978, -354.7018910364275257, -35.00000000000000000 ) ) ;
#9759 = CARTESIAN_POINT ( 'NONE',  ( 145.5008360144876747, 198.5836349573982886, 14.00000000000001776 ) ) ;
#9760 = CARTESIAN_POINT ( 'NONE',  ( -159.5594255724347761, -191.7891397928654555, 43.77915905869157598 ) ) ;
#9761 = ADVANCED_FACE ( 'NONE', ( #8596 ), #20280, .F. ) ;
#9762 = DIRECTION ( 'NONE',  ( 0.000000000000000000, -1.000000000000000000, 0.000000000000000000 ) ) ;
#9763 = DIRECTION ( 'NONE',  ( -0.000000000000000000, 1.000000000000000000, -0.000000000000000000 ) ) ;
#9764 = CARTESIAN_POINT ( 'NONE',  ( -157.2955611005346270, -193.4438272943106938, 57.67623309621198047 ) ) ;
#9765 = CONTEXT_DEPENDENT_SHAPE_REPRESENTATION ( #11966, #2708 ) ;
#9766 = CARTESIAN_POINT ( 'NONE',  ( 38.96631938032478359, 126.0844580088725735, 37.14960608071593384 ) ) ;
#9767 = CARTESIAN_POINT ( 'NONE',  ( 46.59305225739526435, 107.1797705074273352, 31.60846029578754468 ) ) ;
#9768 = CARTESIAN_POINT ( 'NONE',  ( 23.10700517764660589, 139.6571016847272233, -10.96257334342637435 ) ) ;
#9769 = CARTESIAN_POINT ( 'NONE',  ( -143.8425227516148084, -183.6938272943107506, 55.19815736654470584 ) ) ;
#9770 = CARTESIAN_POINT ( 'NONE',  ( 40.27526882409969744, 90.56518717409400665, 37.97664729208901235 ) ) ;
#9771 = EDGE_CURVE ( 'NONE', #4775, #2592, #5387, .T. ) ;
#9772 = FACE_OUTER_BOUND ( 'NONE', #3892, .T. ) ;
#9773 = ORIENTED_EDGE ( 'NONE', *, *, #18784, .F. ) ;
#9774 = CARTESIAN_POINT ( 'NONE',  ( 42.21948215057683740, 138.4575765865523067, 39.21067981925357060 ) ) ;
#9775 = CARTESIAN_POINT ( 'NONE',  ( 38.54497605562327323, 85.96704844161884296, 14.48200433579215662 ) ) ;
#9776 = VECTOR ( 'NONE', #14376, 1000.000000000000000 ) ;
#9777 = CARTESIAN_POINT ( 'NONE',  ( 32.23767430054685690, 145.5917660130465379, 17.43780275515692679 ) ) ;
#9778 = CARTESIAN_POINT ( 'NONE',  ( 46.59305225739526435, 65.17977050742732104, 31.60846029578754468 ) ) ;
#9779 = ORIENTED_EDGE ( 'NONE', *, *, #7673, .T. ) ;
#9780 = ORIENTED_EDGE ( 'NONE', *, *, #17590, .F. ) ;
#9781 = CARTESIAN_POINT ( 'NONE',  ( 39.42975644700377558, 150.0797705074273267, 31.60846029578754468 ) ) ;
#9782 = PLANE ( 'NONE',  #1032 ) ;
#9783 = EDGE_CURVE ( 'NONE', #10801, #470, #6433, .T. ) ;
#9784 = CARTESIAN_POINT ( 'NONE',  ( 39.92123440845004723, 111.2604996726487343, 29.95742577749337343 ) ) ;
#9785 = CARTESIAN_POINT ( 'NONE',  ( 43.01140435219951286, 71.36518717409397539, 29.55568802177586463 ) ) ;
#9786 = CARTESIAN_POINT ( 'NONE',  ( 0.000000000000000000, -37.13255853780189852, -35.00000000000000000 ) ) ;
#9787 = CARTESIAN_POINT ( 'NONE',  ( -143.8425227516148084, -159.0938272943107279, 44.11586579668791330 ) ) ;
#9788 = CIRCLE ( 'NONE', #17853, 7.500000000000007105 ) ;
#9789 = CARTESIAN_POINT ( 'NONE',  ( -124.3720331620955619, 13.78046159333444720, -19.99999999999997868 ) ) ;
#9790 = CARTESIAN_POINT ( 'NONE',  ( -157.6495955161842062, -181.1130981290893089, 58.16351966513671812 ) ) ;
#9791 = CYLINDRICAL_SURFACE ( 'NONE', #5442, 4.999999999999997335 ) ;
#9792 = CARTESIAN_POINT ( 'NONE',  ( 38.01140435219951996, 152.6344580088725422, 32.58608133808903773 ) ) ;
#9793 = CARTESIAN_POINT ( 'NONE',  ( 40.27526882409969033, 132.8297705074273267, 37.97664729208901946 ) ) ;
#9794 =( BOUNDED_CURVE ( )  B_SPLINE_CURVE ( 2, ( #18350, #13392, #9982, #11841, #15263, #6892, #13599, #20338, #11949, #18679, #3582, #5869, #4007 ),
 .UNSPECIFIED., .F., .F. ) 
 B_SPLINE_CURVE_WITH_KNOTS ( ( 3, 2, 2, 2, 2, 2, 3 ),
 ( 0.5955882352941176405, 0.5970588235294117530, 0.5999999999999999778, 0.6029411764705882026, 0.6058823529411764275, 0.6088235294117646523, 0.6102941176470587648 ),
 .UNSPECIFIED. ) 
 CURVE ( )  GEOMETRIC_REPRESENTATION_ITEM ( )  RATIONAL_B_SPLINE_CURVE ( ( 0.9755282581475768211, 0.9755282581475768211, 1.000000000000000000, 0.9510565162951535312, 1.000000000000000000, 0.9510565162951535312, 1.000000000000000000, 0.9510565162951535312, 1.000000000000000000, 0.9510565162951535312, 1.000000000000000000, 0.9755282581475777093, 0.9755282581475768211 ) ) 
 REPRESENTATION_ITEM ( '' )  );
#9795 = CARTESIAN_POINT ( 'NONE',  ( 47.97332496630577481, 153.8600623441721211, 10.00146007428102379 ) ) ;
#9796 = CARTESIAN_POINT ( 'NONE',  ( 47.43856463449117911, 112.7651871740940379, 32.77220824515697473 ) ) ;
#9797 = CARTESIAN_POINT ( 'NONE',  ( -154.5594255724347761, -183.0891397928654669, 40.14644641866476604 ) ) ;
#9798 = CARTESIAN_POINT ( 'NONE',  ( -159.0959885057557983, -158.4584106276440423, 44.11586579668791330 ) ) ;
#9799 = DIRECTION ( 'NONE',  ( -0.000000000000000000, -1.000000000000000000, -0.000000000000000000 ) ) ;
#9800 = CARTESIAN_POINT ( 'NONE',  ( 53.48172298457406271, 87.39834721931525507, 0.9865115032505324955 ) ) ;
#9801 = EDGE_CURVE ( 'NONE', #6227, #4859, #12213, .T. ) ;
#9802 = CARTESIAN_POINT ( 'NONE',  ( 65.96530660583994177, 103.3855952397044007, 19.36639486037446289 ) ) ;
#9803 = DIRECTION ( 'NONE',  ( 0.000000000000000000, 0.000000000000000000, 1.000000000000000000 ) ) ;
#9804 = CARTESIAN_POINT ( 'NONE',  ( 45.74753988029934249, 91.42977050742732104, 37.97664729208901235 ) ) ;
#9805 = VERTEX_POINT ( 'NONE', #18948 ) ;
#9806 = CARTESIAN_POINT ( 'NONE',  ( -148.3790856849358306, -167.4630981290893033, 40.14644641866477315 ) ) ;
#9807 = ORIENTED_EDGE ( 'NONE', *, *, #15169, .T. ) ;
#9808 = CARTESIAN_POINT ( 'NONE',  ( 43.01140435219951286, 104.0344580088725763, 29.21067981925356705 ) ) ;
#9809 = CARTESIAN_POINT ( 'NONE',  ( 39.92123440845004723, 144.2604996726487343, 29.95742577749337343 ) ) ;
#9811 = CARTESIAN_POINT ( 'NONE',  ( 19.47480796662762970, 104.5210170170265229, 9.517959287447121497 ) ) ;
#9810 = CARTESIAN_POINT ( 'NONE',  ( 39.42975644700377558, 98.81518717409400665, 31.60846029578754468 ) ) ;
#9812 = CARTESIAN_POINT ( 'NONE',  ( -157.2955611005346270, -164.6084106276440764, 41.63779006702063867 ) ) ;
#9813 = CARTESIAN_POINT ( 'NONE',  ( -142.0420953463935803, -189.5438272943107165, 52.72008163687743831 ) ) ;
#9814 = DIRECTION ( 'NONE',  ( -0.000000000000000000, -0.000000000000000000, -1.000000000000000000 ) ) ;
#9815 = CARTESIAN_POINT ( 'NONE',  ( 116.4417310231185780, -126.9891397928655010, 30.00000000000000000 ) ) ;
#9816 = LINE ( 'NONE', #20178, #5167 ) ;
#9817 = CARTESIAN_POINT ( 'NONE',  ( 39.42975644700377558, 60.41518717409400097, 36.81289934271958941 ) ) ;
#9818 = CARTESIAN_POINT ( 'NONE',  ( -151.4692556286852891, -185.3130981290893260, 39.65701158161630246 ) ) ;
#9819 = CARTESIAN_POINT ( 'NONE',  ( 26.90790578767411390, 150.1165885900122987, 3.291480155758420345 ) ) ;
#9820 = CARTESIAN_POINT ( 'NONE',  ( 39.42975644700377558, 141.4151871740940010, 36.81289934271958941 ) ) ;
#9821 = CARTESIAN_POINT ( 'NONE',  ( -145.6429501568359797, -162.8438272943107279, 57.67623309621198047 ) ) ;
#9822 = CARTESIAN_POINT ( 'NONE',  ( -151.4692556286852891, -184.4084106276440309, 59.56931450028537256 ) ) ;
#9823 = ORIENTED_EDGE ( 'NONE', *, *, #12708, .F. ) ;
#9824 = CARTESIAN_POINT ( 'NONE',  ( 46.59305225739526435, 70.31518717409400665, 36.81289934271958941 ) ) ;
#9825 = CARTESIAN_POINT ( 'NONE',  ( -143.8425227516148084, -171.3584106276440764, 44.11586579668791330 ) ) ;
#9826 = CARTESIAN_POINT ( 'NONE',  ( 24.18607167610233333, 148.5957190367184353, 16.19189608183989648 ) ) ;
#9827 = CARTESIAN_POINT ( 'NONE',  ( 45.74753988029933538, 121.1651871740939725, 37.97664729208901946 ) ) ;
#9828 = CARTESIAN_POINT ( 'NONE',  ( 58.10477600886401461, 150.5438954262070581, -8.656458923931941385 ) ) ;
#9829 = ORIENTED_EDGE ( 'NONE', *, *, #12154, .F. ) ;
#9830 = VERTEX_POINT ( 'NONE', #5593 ) ;
#9831 = EDGE_CURVE ( 'NONE', #6147, #17644, #5174, .T. ) ;
#9832 = CARTESIAN_POINT ( 'NONE',  ( -141.4692556286852891, -192.8391397928654669, 46.40781461928724383 ) ) ;
#9833 = ORIENTED_EDGE ( 'NONE', *, *, #6546, .T. ) ;
#9834 = CARTESIAN_POINT ( 'NONE',  ( -130.4480969619997950, -136.9891397928655010, -72.64809332337412684 ) ) ;
#9835 = AXIS2_PLACEMENT_3D ( 'NONE', #11221, #19827, #21488 ) ;
#9836 = CARTESIAN_POINT ( 'NONE',  ( 47.43856463449117200, 70.72977050742730398, 35.64915139335016647 ) ) ;
#9838 = CARTESIAN_POINT ( 'NONE',  ( 40.57367117788501787, 91.81261228707245436, 0.5136478283763052932 ) ) ;
#9837 = CARTESIAN_POINT ( 'NONE',  ( 45.74753988029933538, 127.1651871740939725, 37.97664729208901946 ) ) ;
#9839 = CARTESIAN_POINT ( 'NONE',  ( 46.10157429594899270, 80.66049967264873999, 29.95742577749337343 ) ) ;
#9840 = CARTESIAN_POINT ( 'NONE',  ( 9.231363607564425422, 125.4582397780895633, 16.26765482522027639 ) ) ;
#9841 = CARTESIAN_POINT ( 'NONE',  ( 38.01140435219952707, 144.5604996726487173, 32.58608133808903773 ) ) ;
#9842 = CARTESIAN_POINT ( 'NONE',  ( 39.92123440845005433, 138.2604996726487343, 29.95742577749336988 ) ) ;
#9843 = CARTESIAN_POINT ( 'NONE',  ( 40.27526882409969033, 84.56518717409397823, 37.97664729208901946 ) ) ;
#9844 = CARTESIAN_POINT ( 'NONE',  ( 48.01140435219951996, 151.4344580088725820, 32.58608133808903773 ) ) ;
#9845 = CARTESIAN_POINT ( 'NONE',  ( -157.6495955161842062, -185.0391397928654271, 58.16351966513671812 ) ) ;
#9846 = VERTEX_POINT ( 'NONE', #3848 ) ;
#9847 = CARTESIAN_POINT ( 'NONE',  ( 44.37947211624943833, 62.47977050742731109, 30.00020018409699318 ) ) ;
#9848 = CARTESIAN_POINT ( 'NONE',  ( -154.3824083646099439, -157.2938272943107449, 58.62277379824867296 ) ) ;
#9849 = CARTESIAN_POINT ( 'NONE',  ( 29.43094928344231320, 88.48265962617873015, 0.7917390523231137012 ) ) ;
#9850 = CARTESIAN_POINT ( 'NONE',  ( -142.0420953463935803, -189.5084106276440536, 46.59394152635518793 ) ) ;
#9851 = ORIENTED_EDGE ( 'NONE', *, *, #12435, .T. ) ;
#9852 = CARTESIAN_POINT ( 'NONE',  ( 47.43856463449118621, 151.6151871740939896, 34.21067981925357060 ) ) ;
#9853 = DIRECTION ( 'NONE',  ( -1.000000000000000000, 0.000000000000000000, 0.000000000000000000 ) ) ;
#9854 = CARTESIAN_POINT ( 'NONE',  ( 41.64333658814960870, 113.7797705074273296, 30.00020018409699318 ) ) ;
#9855 = CARTESIAN_POINT ( 'NONE',  ( 44.41273964558330789, 85.70220254879866673, -6.708519844216274564 ) ) ;
#9856 = ORIENTED_EDGE ( 'NONE', *, *, #9461, .F. ) ;
#9857 = CARTESIAN_POINT ( 'NONE',  ( 48.01140435219951996, 88.43445800887258201, 32.58608133808903773 ) ) ;
#9858 = ORIENTED_EDGE ( 'NONE', *, *, #121, .T. ) ;
#9859 = CARTESIAN_POINT ( 'NONE',  ( 47.43856463449117200, 116.0297705074273154, 32.77220824515698183 ) ) ;
#9860 = CARTESIAN_POINT ( 'NONE',  ( 39.92123440845005433, 72.26049967264872009, 29.95742577749336988 ) ) ;
#9861 = CARTESIAN_POINT ( 'NONE',  ( 45.74753988029933538, 85.42977050742730682, 37.97664729208901946 ) ) ;
#9862 = CARTESIAN_POINT ( 'NONE',  ( 44.37947211624943833, 157.0151871740940237, 38.42115945441014446 ) ) ;
#9863 = EDGE_CURVE ( 'NONE', #5083, #3809, #13758, .T. ) ;
#9864 = PRODUCT_DEFINITION_FORMATION_WITH_SPECIFIED_SOURCE ( 'ANY', '', #19990, .NOT_KNOWN. ) ;
#9865 = DIRECTION ( 'NONE',  ( -0.9999746145782334450, 0.007125320983193089534, 0.000000000000000000 ) ) ;
#9866 = PLANE ( 'NONE',  #18383 ) ;
#9867 = CARTESIAN_POINT ( 'NONE',  ( -145.2889157411863721, -183.5391397928655124, 41.15050349809590102 ) ) ;
#9868 = CARTESIAN_POINT ( 'NONE',  ( 148.6725454929228079, -61.68114226949890622, 19.99999999999998934 ) ) ;
#9869 = CARTESIAN_POINT ( 'NONE',  ( 46.10157429594899270, 131.6604996726487400, 29.95742577749336988 ) ) ;
#9870 = CARTESIAN_POINT ( 'NONE',  ( -142.0420953463935803, -189.2438272943107336, 46.59394152635518793 ) ) ;
#9871 = CARTESIAN_POINT ( 'NONE',  ( 46.10157429594899270, 121.7344580088725792, 29.95742577749337343 ) ) ;
#9872 = CARTESIAN_POINT ( 'NONE',  ( 44.37947211624943833, 95.47977050742731819, 30.00020018409699318 ) ) ;
#9873 = CARTESIAN_POINT ( 'NONE',  ( 26.61521700243209310, 142.9206948758876194, 23.22567064538713666 ) ) ;
#9874 = CARTESIAN_POINT ( 'NONE',  ( -148.5561028927606344, -183.9938272943107336, 58.62277379824867296 ) ) ;
#9875 = CARTESIAN_POINT ( 'NONE',  ( 40.27526882409969744, 89.66518717409400097, 30.44471234641812174 ) ) ;
#9876 = LINE ( 'NONE', #3694, #6556 ) ;
#9877 = ORIENTED_EDGE ( 'NONE', *, *, #21484, .F. ) ;
#9878 = FACE_OUTER_BOUND ( 'NONE', #6321, .T. ) ;
#9879 = ADVANCED_FACE ( 'NONE', ( #12320 ), #3635, .T. ) ;
#9880 = CARTESIAN_POINT ( 'NONE',  ( 31.47436479266152531, 87.67613096727390598, 14.72005176623422606 ) ) ;
#9881 = CARTESIAN_POINT ( 'NONE',  ( 47.43856463449118621, 145.8797705074273097, 34.21067981925357060 ) ) ;
#9882 = CARTESIAN_POINT ( 'NONE',  ( 38.46765184765857981, 147.6574975633170936, -2.267929528491105629 ) ) ;
#9883 = CARTESIAN_POINT ( 'NONE',  ( 47.43856463449118621, 106.6151871740940038, 34.21067981925357060 ) ) ;
#9884 = CARTESIAN_POINT ( 'NONE',  ( 40.27526882409969744, 69.82977050742731251, 37.97664729208901235 ) ) ;
#9885 = EDGE_LOOP ( 'NONE', ( #8641, #14747 ) ) ;
#9886 = EDGE_CURVE ( 'NONE', #18762, #1989, #8115, .T. ) ;
#9887 = CARTESIAN_POINT ( 'NONE',  ( 44.37947211624943833, 148.2797705074273154, 38.42115945441014446 ) ) ;
#9888 = CARTESIAN_POINT ( 'NONE',  ( 43.01140435219951286, 97.12977050742732388, 38.86567161673127657 ) ) ;
#9889 = FACE_BOUND ( 'NONE', #6544, .T. ) ;
#9890 = CARTESIAN_POINT ( 'NONE',  ( 38.01140435219952707, 114.7104996726487371, 34.21067981925357060 ) ) ;
#9891 = CARTESIAN_POINT ( 'NONE',  ( 43.01140435219951286, 72.86518717409400381, 38.86567161673127657 ) ) ;
#9892 = DIRECTION ( 'NONE',  ( 0.000000000000000000, 0.000000000000000000, 1.000000000000000000 ) ) ;
#9893 = CARTESIAN_POINT ( 'NONE',  ( -160.8964159109769696, -157.8938272943107393, 49.65701158161630957 ) ) ;
#9894 = CARTESIAN_POINT ( 'NONE',  ( 163.1866912085270371, 192.1987543186987466, 19.40769008390923389 ) ) ;
#9895 = CARTESIAN_POINT ( 'NONE',  ( -143.3790856849358306, -176.7630981290893146, 43.77915905869157598 ) ) ;
#9896 = CARTESIAN_POINT ( 'NONE',  ( 43.01140435219954838, 110.9604996726487371, 29.21067981925356705 ) ) ;
#9897 = CARTESIAN_POINT ( 'NONE',  ( 48.01140435219951996, 148.2844580088725763, 34.21067981925357060 ) ) ;
#9898 = CARTESIAN_POINT ( 'NONE',  ( 41.64333658814960870, 131.7797705074273154, 30.00020018409699318 ) ) ;
#9899 = CARTESIAN_POINT ( 'NONE',  ( 75.73800832010900308, 109.5907576069244698, 18.92991194937467014 ) ) ;
#9900 = CARTESIAN_POINT ( 'NONE',  ( 39.42975644700377558, 113.8151871740940067, 31.60846029578754468 ) ) ;
#9901 = CARTESIAN_POINT ( 'NONE',  ( 149.5529451524149920, 187.4828467975320336, 14.00000000000001776 ) ) ;
#9902 = FACE_OUTER_BOUND ( 'NONE', #5343, .T. ) ;
#9903 = DIRECTION ( 'NONE',  ( 0.000000000000000000, 0.000000000000000000, -1.000000000000000000 ) ) ;
#9904 = CARTESIAN_POINT ( 'NONE',  ( 68.08897506277223499, 96.72110655255949041, 7.414802352519190620 ) ) ;
#9905 = CARTESIAN_POINT ( 'NONE',  ( 55.29376081731632553, 145.2908078538121401, -2.581636314160848489 ) ) ;
#9906 = CARTESIAN_POINT ( 'NONE',  ( -151.4692556286852891, -196.9891397928655010, 49.65701158161630957 ) ) ;
#9907 = CARTESIAN_POINT ( 'NONE',  ( 44.37947211624943833, 95.47977050742731819, 30.00020018409699318 ) ) ;
#9908 = EDGE_LOOP ( 'NONE', ( #11493, #21655, #11523, #16892 ) ) ;
#9909 = DIRECTION ( 'NONE',  ( 0.4683024526015100442, -0.8835682276357670339, 0.000000000000000000 ) ) ;
#9910 = VERTEX_POINT ( 'NONE', #17171 ) ;
#9911 = CARTESIAN_POINT ( 'NONE',  ( 47.05648932407426344, 85.58445800887258770, 31.27175355779120025 ) ) ;
#9912 = LINE ( 'NONE', #16503, #18987 ) ;
#9913 = CARTESIAN_POINT ( 'NONE',  ( 41.46631938032478359, 142.3104996726487457, 38.96596240072933170 ) ) ;
#9915 = CARTESIAN_POINT ( 'NONE',  ( 70.62278752756289180, 114.5844828164671441, -0.1247842873985126749 ) ) ;
#9914 = CARTESIAN_POINT ( 'NONE',  ( 47.43856463449118621, 94.61518717409400381, 34.21067981925357060 ) ) ;
#9916 =( BOUNDED_CURVE ( )  B_SPLINE_CURVE ( 2, ( #10249, #16948, #2184, #12209, #10141, #18724, #16844, #6943, #1757, #8492, #13649, #18944, #10571 ),
 .UNSPECIFIED., .F., .F. ) 
 B_SPLINE_CURVE_WITH_KNOTS ( ( 3, 2, 2, 2, 2, 2, 3 ),
 ( 0.6397058823529411242, 0.6411764705882353477, 0.6441176470588235725, 0.6470588235294117974, 0.6500000000000000222, 0.6529411764705882470, 0.6544117647058823595 ),
 .UNSPECIFIED. ) 
 CURVE ( )  GEOMETRIC_REPRESENTATION_ITEM ( )  RATIONAL_B_SPLINE_CURVE ( ( 0.9755282581475768211, 0.9755282581475758219, 1.000000000000000000, 0.9510565162951535312, 1.000000000000000000, 0.9510565162951535312, 1.000000000000000000, 0.9510565162951535312, 1.000000000000000000, 0.9510565162951535312, 1.000000000000000000, 0.9755282581475768211, 0.9755282581475768211 ) ) 
 REPRESENTATION_ITEM ( '' )  );
#9917 = EDGE_CURVE ( 'NONE', #19197, #2548, #8829, .T. ) ;
#9918 = CARTESIAN_POINT ( 'NONE',  ( -160.8964159109769696, -170.3084106276440082, 46.59394152635518793 ) ) ;
#9919 = CARTESIAN_POINT ( 'NONE',  ( -145.6429501568359797, -186.8438272943106995, 57.67623309621197336 ) ) ;
#9921 = LINE ( 'NONE', #18508, #16407 ) ;
#9920 = CARTESIAN_POINT ( 'NONE',  ( -154.5594255724347761, -179.1630981290893203, 40.14644641866476604 ) ) ;
#9922 = DIRECTION ( 'NONE',  ( -1.000000000000000000, 0.000000000000000000, 0.000000000000000000 ) ) ;
#9923 = CIRCLE ( 'NONE', #20482, 7.500000000000000000 ) ;
#9924 = CARTESIAN_POINT ( 'NONE',  ( -149.8854112254399809, -174.3160212151857422, 39.65701158161628825 ) ) ;
#9925 = CARTESIAN_POINT ( 'NONE',  ( 38.01140435219952707, 78.71049967264875136, 34.21067981925357060 ) ) ;
#9926 = CARTESIAN_POINT ( 'NONE',  ( 41.64333658814960870, 59.51518717409400239, 30.00020018409699318 ) ) ;
#9927 = CARTESIAN_POINT ( 'NONE',  ( 38.01140435219952707, 62.93445800887258201, 35.83527830041809636 ) ) ;
#9928 = CARTESIAN_POINT ( 'NONE',  ( 25.52397925108762067, 90.47728371212039633, 7.934596195134201224 ) ) ;
#9929 = CARTESIAN_POINT ( 'NONE',  ( 46.59305225739526435, 142.3151871740940067, 36.81289934271958941 ) ) ;
#9930 = CARTESIAN_POINT ( 'NONE',  ( -143.8425227516148084, -159.6938272943107222, 55.19815736654470584 ) ) ;
#9931 = CARTESIAN_POINT ( 'NONE',  ( -142.0420953463935803, -171.5084106276440536, 46.59394152635518083 ) ) ;
#9932 = EDGE_CURVE ( 'NONE', #20322, #16938, #11483, .T. ) ;
#9933 = ORIENTED_EDGE ( 'NONE', *, *, #19774, .F. ) ;
#9934 = CARTESIAN_POINT ( 'NONE',  ( 44.82204145925543060, 59.16666223754088350, 30.14399968058850021 ) ) ;
#9935 = CARTESIAN_POINT ( 'NONE',  ( -154.3824083646099439, -157.5584106276440650, 58.62277379824867296 ) ) ;
#9936 = CARTESIAN_POINT ( 'NONE',  ( 76.97284262070103011, 124.8108046395131225, 11.43003150283799663 ) ) ;
#9937 = CARTESIAN_POINT ( 'NONE',  ( 38.58424406990784661, 125.9651871740939697, 32.77220824515698183 ) ) ;
#9938 = CARTESIAN_POINT ( 'NONE',  ( 69.07271358049158039, 97.83220508185358710, -6.632443479277712051 ) ) ;
#9939 = ORIENTED_EDGE ( 'NONE', *, *, #2982, .F. ) ;
#9940 = ORIENTED_EDGE ( 'NONE', *, *, #11768, .T. ) ;
#9941 = AXIS2_PLACEMENT_3D ( 'NONE', #12573, #21071, #459 ) ;
#9942 = VECTOR ( 'NONE', #11004, 1000.000000000000000 ) ;
#9943 = DIRECTION ( 'NONE',  ( -0.3428981916074324565, 0.9393725726208703719, 0.000000000000000000 ) ) ;
#9944 = EDGE_LOOP ( 'NONE', ( #7097, #15565, #6347, #19492 ) ) ;
#9945 = CARTESIAN_POINT ( 'NONE',  ( 43.01140435219951286, 115.4604996726487229, 39.21067981925356349 ) ) ;
#9946 = VECTOR ( 'NONE', #4296, 1000.000000000000000 ) ;
#9947 = CARTESIAN_POINT ( 'NONE',  ( 46.59305225739526435, 65.17977050742732104, 31.60846029578754468 ) ) ;
#9949 = CARTESIAN_POINT ( 'NONE',  ( 19.23080508249268661, 135.0620028898917440, 9.799277925644819476 ) ) ;
#9948 = CARTESIAN_POINT ( 'NONE',  ( 47.43856463449117200, 121.4651871740939839, 35.64915139335016647 ) ) ;
#9950 = CARTESIAN_POINT ( 'NONE',  ( 41.46631938032478359, 79.31049967264873146, 38.96596240072933170 ) ) ;
#9951 = DIRECTION ( 'NONE',  ( 0.9385982292947087080, 0.3450121214752278620, -1.836742322155470738E-16 ) ) ;
#9952 = CARTESIAN_POINT ( 'NONE',  ( 44.55648932407425633, 97.61049967264874283, 38.96596240072933170 ) ) ;
#9953 = DIRECTION ( 'NONE',  ( 1.000000000000000000, 0.000000000000000000, 0.000000000000000000 ) ) ;
#9954 = CARTESIAN_POINT ( 'NONE',  ( 39.42975644700377558, 83.81518717409400665, 31.60846029578754468 ) ) ;
#9955 = CARTESIAN_POINT ( 'NONE',  ( 38.01140435219952707, 81.86049967264874283, 35.83527830041809636 ) ) ;
#9956 = PRODUCT ( 'Upper Movable Curved Shear Blade', 'Upper Movable Curved Shear Blade', '', ( #16687 ) ) ;
#9957 = CYLINDRICAL_SURFACE ( 'NONE', #16605, 10.00000000000000888 ) ;
#9958 = EDGE_CURVE ( 'NONE', #21594, #17127, #15571, .T. ) ;
#9959 = VERTEX_POINT ( 'NONE', #5709 ) ;
#9960 = CARTESIAN_POINT ( 'NONE',  ( 47.43856463449118621, 64.87977050742730967, 34.21067981925357060 ) ) ;
#9961 = CARTESIAN_POINT ( 'NONE',  ( -151.4692556286852891, -185.9084106276440025, 39.74470866294723947 ) ) ;
#9962 = CARTESIAN_POINT ( 'NONE',  ( 73.72238702602700755, 135.0318370961144296, 5.077453337991364002 ) ) ;
#9963 = CARTESIAN_POINT ( 'NONE',  ( -159.0959885057557983, -185.4584106276440707, 44.11586579668791330 ) ) ;
#9964 = ORIENTED_EDGE ( 'NONE', *, *, #8119, .T. ) ;
#9965 = CARTESIAN_POINT ( 'NONE',  ( 43.01140435219951286, 152.3651871740940180, 29.55568802177586463 ) ) ;
#9966 = CARTESIAN_POINT ( 'NONE',  ( 43.01140435219951286, 61.46049967264873715, 39.21067981925356349 ) ) ;
#9967 = CARTESIAN_POINT ( 'NONE',  ( 38.58424406990785371, 114.5297705074273296, 35.64915139335015937 ) ) ;
#9968 = CARTESIAN_POINT ( 'NONE',  ( 76.04618105687035268, 128.8835079444423286, -1.708432735116285350 ) ) ;
#9969 = ORIENTED_EDGE ( 'NONE', *, *, #11352, .F. ) ;
#9970 = CARTESIAN_POINT ( 'NONE',  ( 20.25093610150840107, 136.5556286039603435, -4.129180435126924564 ) ) ;
#9971 = ORIENTED_EDGE ( 'NONE', *, *, #18784, .T. ) ;
#9972 = CARTESIAN_POINT ( 'NONE',  ( 38.58424406990786082, 114.3797705074273097, 34.21067981925357060 ) ) ;
#9973 = DIRECTION ( 'NONE',  ( 0.000000000000000000, 0.000000000000000000, 1.000000000000000000 ) ) ;
#9974 = CARTESIAN_POINT ( 'NONE',  ( 45.74753988029933538, 151.1651871740939725, 37.97664729208901946 ) ) ;
#9975 = CARTESIAN_POINT ( 'NONE',  ( 60.49690154327523572, 149.3382625450468311, -9.565656633516235630 ) ) ;
#9976 = DIRECTION ( 'NONE',  ( 1.000000000000000000, 0.000000000000000000, 0.000000000000000000 ) ) ;
#9977 = CARTESIAN_POINT ( 'NONE',  ( 48.01140435219951996, 82.28445800887257633, 34.21067981925357060 ) ) ;
#9978 = DIRECTION ( 'NONE',  ( -0.2767211344570352782, 0.9609502660100632809, 0.000000000000000000 ) ) ;
#9979 = CARTESIAN_POINT ( 'NONE',  ( -159.5594255724347761, -176.7891397928654840, 43.77915905869157598 ) ) ;
#9980 = LINE ( 'NONE', #1262, #18584 ) ;
#9981 = CARTESIAN_POINT ( 'NONE',  ( 43.01140435219954838, 131.9604996726487229, 29.21067981925356705 ) ) ;
#9982 = CARTESIAN_POINT ( 'NONE',  ( 44.55648932407425633, 97.88445800887257064, 29.45539723777780239 ) ) ;
#9983 = ITEM_DEFINED_TRANSFORMATION ( 'NONE', 'NONE', #5635,  #12657 ) ;
#9984 = CARTESIAN_POINT ( 'NONE',  ( 43.01140435219951286, 95.62977050742732388, 29.55568802177586463 ) ) ;
#9985 =( BOUNDED_CURVE ( )  B_SPLINE_CURVE ( 2, ( #17656, #1238, #6193, #18207, #4759, #13143, #14680, #6084, #11595, #7973, #21531, #12812, #18324 ),
 .UNSPECIFIED., .F., .F. ) 
 B_SPLINE_CURVE_WITH_KNOTS ( ( 3, 2, 2, 2, 2, 2, 3 ),
 ( 0.1544117647058823595, 0.1558823529411764719, 0.1588235294117646967, 0.1617647058823529493, 0.1647058823529411742, 0.1676470588235293990, 0.1691176470588235115 ),
 .UNSPECIFIED. ) 
 CURVE ( )  GEOMETRIC_REPRESENTATION_ITEM ( )  RATIONAL_B_SPLINE_CURVE ( ( 0.9755282581475768211, 0.9755282581475768211, 1.000000000000000000, 0.9510565162951535312, 1.000000000000000000, 0.9510565162951535312, 1.000000000000000000, 0.9510565162951535312, 1.000000000000000000, 0.9510565162951535312, 1.000000000000000000, 0.9755282581475769321, 0.9755282581475765991 ) ) 
 REPRESENTATION_ITEM ( '' )  );
#9986 = CARTESIAN_POINT ( 'NONE',  ( 71.28758990370504023, 120.3962046462169440, 18.65202787790538608 ) ) ;
#9987 = CARTESIAN_POINT ( 'NONE',  ( -154.3824083646099439, -184.2938272943107449, 58.62277379824867296 ) ) ;
#9988 = CARTESIAN_POINT ( 'NONE',  ( 39.42975644700377558, 83.81518717409400665, 31.60846029578754468 ) ) ;
#9989 = DIRECTION ( 'NONE',  ( 0.3428981916074309577, -0.9393725726208709270, 0.000000000000000000 ) ) ;
#9990 = ORIENTED_EDGE ( 'NONE', *, *, #17001, .F. ) ;
#9991 = VECTOR ( 'NONE', #11474, 1000.000000000000000 ) ;
#9992 = FACE_OUTER_BOUND ( 'NONE', #2933, .T. ) ;
#9993 = CARTESIAN_POINT ( 'NONE',  ( 41.61242760320212852, 154.1118385459532760, 10.79173905232880237 ) ) ;
#9994 = CARTESIAN_POINT ( 'NONE',  ( 71.07673676950255981, 118.1590465568689581, -7.267641430287227422 ) ) ;
#9995 = CARTESIAN_POINT ( 'NONE',  ( 135.5718357590524192, 174.6787949867965324, 14.00000000000001776 ) ) ;
#9996 = ORIENTED_EDGE ( 'NONE', *, *, #20323, .F. ) ;
#9997 = CARTESIAN_POINT ( 'NONE',  ( 47.43856463449117200, 145.7297705074272756, 35.64915139335016647 ) ) ;
#9998 = CARTESIAN_POINT ( 'NONE',  ( 46.59305225739526435, 98.17977050742732104, 31.60846029578754468 ) ) ;
#9999 = ADVANCED_FACE ( 'NONE', ( #20928 ), #11101, .F. ) ;
#10000 = CARTESIAN_POINT ( 'NONE',  ( -151.4692556286852891, -196.9891397928655010, 49.65701158161630957 ) ) ;
#10001 = CARTESIAN_POINT ( 'NONE',  ( 48.01140435219951996, 113.0604996726487457, 35.83527830041810347 ) ) ;
#10002 = CARTESIAN_POINT ( 'NONE',  ( 43.01140435219951286, 66.86518717409397539, 38.86567161673127657 ) ) ;
#10003 = DIRECTION ( 'NONE',  ( 0.000000000000000000, 0.000000000000000000, 1.000000000000000000 ) ) ;
#10004 = CARTESIAN_POINT ( 'NONE',  ( -142.0420953463936087, -165.3938272943107393, 49.65701158161630957 ) ) ;
#10005 = CARTESIAN_POINT ( 'NONE',  ( 38.96631938032478359, 155.4844580088725934, 31.27175355779120025 ) ) ;
#10006 = CARTESIAN_POINT ( 'NONE',  ( -151.4692556286852891, -182.3130981290893260, 39.14238933923362396 ) ) ;
#10007 = CARTESIAN_POINT ( 'NONE',  ( 41.46631938032478359, 152.1844580088725820, 29.45539723777780239 ) ) ;
#10008 = CARTESIAN_POINT ( 'NONE',  ( 43.01140435219951286, 119.6297705074272955, 29.55568802177586463 ) ) ;
#10009 = CARTESIAN_POINT ( 'NONE',  ( 76.97284262070103011, 124.8108046395131225, 11.43003150283799663 ) ) ;
#10010 = DIRECTION ( 'NONE',  ( -0.5573926701119628069, 0.8302490056034133037, 0.000000000000000000 ) ) ;
#10011 = CARTESIAN_POINT ( 'NONE',  ( 43.01140435219951286, 119.3651871740940038, 29.55568802177586107 ) ) ;
#10012 = DIRECTION ( 'NONE',  ( 0.000000000000000000, 0.000000000000000000, 1.000000000000000000 ) ) ;
#10013 = FACE_OUTER_BOUND ( 'NONE', #15877, .T. ) ;
#10014 = CARTESIAN_POINT ( 'NONE',  ( 75.39856087065255963, 130.7497677300756607, 6.224699377836747871 ) ) ;
#10015 = CARTESIAN_POINT ( 'NONE',  ( 27.10205971394288582, 96.62443569844734270, -5.915007788698968483 ) ) ;
#10016 = CARTESIAN_POINT ( 'NONE',  ( -151.4692556286852891, -186.8130981290893260, 59.65701158161632378 ) ) ;
#10017 = CARTESIAN_POINT ( 'NONE',  ( 41.64333658814960870, 96.97977050742731819, 38.42115945441014446 ) ) ;
#10018 = CIRCLE ( 'NONE', #9309, 10.00000000000000888 ) ;
#10019 = ORIENTED_EDGE ( 'NONE', *, *, #16809, .T. ) ;
#10020 = LINE ( 'NONE', #1417, #4147 ) ;
#10021 = ORIENTED_EDGE ( 'NONE', *, *, #21370, .T. ) ;
#10022 = CARTESIAN_POINT ( 'NONE',  ( 41.46631938032478359, 83.18445800887258201, 29.45539723777780239 ) ) ;
#10023 = CARTESIAN_POINT ( 'NONE',  ( 39.92123440845005433, 60.23445800887256496, 38.46393386101375711 ) ) ;
#10024 = CARTESIAN_POINT ( 'NONE',  ( 38.96631938032478359, 142.0104996726487627, 37.14960608071593384 ) ) ;
#10026 = CARTESIAN_POINT ( 'NONE',  ( 69.49278103613195867, 129.3669923906968222, -0.7201859908431552659 ) ) ;
#10025 = CARTESIAN_POINT ( 'NONE',  ( 43.01140435219951286, 101.3651871740939896, 29.55568802177586463 ) ) ;
#10027 = CARTESIAN_POINT ( 'NONE',  ( -145.6429501568359797, -168.2084106276440139, 41.63779006702063867 ) ) ;
#10028 = CARTESIAN_POINT ( 'NONE',  ( -160.8964159109769696, -193.7438272943107052, 52.72008163687743121 ) ) ;
#10030 = CARTESIAN_POINT ( 'NONE',  ( -97.23064952102208736, 13.78046159333444720, 4.000000000000021316 ) ) ;
#10029 = CYLINDRICAL_SURFACE ( 'NONE', #5518, 24.99999999999998934 ) ;
#10031 = CARTESIAN_POINT ( 'NONE',  ( 41.46631938032478359, 105.1104996726487428, 29.45539723777780239 ) ) ;
#10032 = EDGE_CURVE ( 'NONE', #9411, #10505, #14406, .T. ) ;
#10033 = CARTESIAN_POINT ( 'NONE',  ( -79.69854755000110913, 605.3054376597395958, -3.999999999999980904 ) ) ;
#10034 = CARTESIAN_POINT ( 'NONE',  ( 48.01140435219951996, 146.2104996726487229, 34.21067981925357060 ) ) ;
#10035 = CARTESIAN_POINT ( 'NONE',  ( 40.27526882409969033, 147.8297705074272983, 37.97664729208901946 ) ) ;
#10036 = DIRECTION ( 'NONE',  ( 1.000000000000000000, 0.000000000000000000, 0.000000000000000000 ) ) ;
#10037 = ADVANCED_FACE ( 'NONE', ( #19159 ), #7809, .F. ) ;
#10038 = CARTESIAN_POINT ( 'NONE',  ( 8.869018199820361659, 117.4101421016551967, 9.005765870029716069 ) ) ;
#10039 = VECTOR ( 'NONE', #15289, 1000.000000000000000 ) ;
#10040 = CARTESIAN_POINT ( 'NONE',  ( 38.58424406990786082, 141.1151871740939896, 34.21067981925357060 ) ) ;
#10041 = CARTESIAN_POINT ( 'NONE',  ( -142.0420953463935803, -165.2438272943107052, 46.59394152635518793 ) ) ;
#10042 = CARTESIAN_POINT ( 'NONE',  ( -160.8964159109769696, -176.3084106276440082, 46.59394152635518083 ) ) ;
#10043 = VERTEX_POINT ( 'NONE', #21255 ) ;
#10044 = CARTESIAN_POINT ( 'NONE',  ( 47.43856463449118621, 61.61518717409400381, 34.21067981925357060 ) ) ;
#10045 = CARTESIAN_POINT ( 'NONE',  ( -142.0420953463935803, -159.5084106276440536, 46.59394152635518793 ) ) ;
#10046 = CARTESIAN_POINT ( 'NONE',  ( 39.80927132972225024, 148.0054509460111660, -4.205104553811644941 ) ) ;
#10047 = CARTESIAN_POINT ( 'NONE',  ( 18.67254549292281496, -61.68114226949890622, 20.00000000000001776 ) ) ;
#10048 = CARTESIAN_POINT ( 'NONE',  ( 45.74753988029933538, 127.1651871740939725, 37.97664729208901946 ) ) ;
#10049 = EDGE_LOOP ( 'NONE', ( #17484, #17664 ) ) ;
#10050 = ORIENTED_EDGE ( 'NONE', *, *, #21369, .F. ) ;
#10051 = CARTESIAN_POINT ( 'NONE',  ( 42.21948215057684450, 113.1113394311928317, 29.21067981925356705 ) ) ;
#10052 = ORIENTED_EDGE ( 'NONE', *, *, #10623, .T. ) ;
#10053 =( BOUNDED_CURVE ( )  B_SPLINE_CURVE ( 2, ( #4565, #9652, #7999, #3027, #11286, #16353, #1263, #17893, #6332, #13058, #13283, #19784, #4677 ),
 .UNSPECIFIED., .F., .F. ) 
 B_SPLINE_CURVE_WITH_KNOTS ( ( 3, 2, 2, 2, 2, 2, 3 ),
 ( 0.5514705882352941568, 0.5529411764705882693, 0.5558823529411764941, 0.5588235294117647189, 0.5617647058823529438, 0.5647058823529411686, 0.5661764705882352811 ),
 .UNSPECIFIED. ) 
 CURVE ( )  GEOMETRIC_REPRESENTATION_ITEM ( )  RATIONAL_B_SPLINE_CURVE ( ( 0.9755282581475768211, 0.9755282581475768211, 1.000000000000000000, 0.9510565162951535312, 1.000000000000000000, 0.9510565162951535312, 1.000000000000000000, 0.9510565162951535312, 1.000000000000000000, 0.9510565162951535312, 1.000000000000000000, 0.9755282581475768211, 0.9755282581475768211 ) ) 
 REPRESENTATION_ITEM ( '' )  );
#10054 = CARTESIAN_POINT ( 'NONE',  ( 41.64333658814960870, 66.97977050742731819, 38.42115945441014446 ) ) ;
#10056 = CARTESIAN_POINT ( 'NONE',  ( 15.66613903973849986, 126.7949701480144711, 9.441967288829692606 ) ) ;
#10055 = CARTESIAN_POINT ( 'NONE',  ( 38.58424406990786082, 123.1151871740940038, 34.21067981925357060 ) ) ;
#10057 = CARTESIAN_POINT ( 'NONE',  ( 38.96631938032478359, 84.41049967264873999, 31.27175355779120025 ) ) ;
#10058 = CYLINDRICAL_SURFACE ( 'NONE', #10076, 10.00000000000000888 ) ;
#10059 = AXIS2_PLACEMENT_3D ( 'NONE', #10870, #17572, #13944 ) ;
#10060 = CARTESIAN_POINT ( 'NONE',  ( 116.4417310231185780, -136.9891397928655010, 19.99999999999999645 ) ) ;
#10061 = CARTESIAN_POINT ( 'NONE',  ( -151.4692556286852891, -126.9891397928655010, -54.65701158161630246 ) ) ;
#10062 = CARTESIAN_POINT ( 'NONE',  ( 38.58424406990784661, 86.96518717409398391, 32.77220824515698183 ) ) ;
#10063 = CARTESIAN_POINT ( 'NONE',  ( 38.45534370351731468, 144.4885014985149496, 32.14446507322553970 ) ) ;
#10064 = CARTESIAN_POINT ( 'NONE',  ( 38.01140435219952707, 132.7104996726487514, 34.21067981925357060 ) ) ;
#10065 = ORIENTED_EDGE ( 'NONE', *, *, #11634, .T. ) ;
#10066 = CARTESIAN_POINT ( 'NONE',  ( 38.58424406990784661, 66.52977050742730114, 35.64915139335016647 ) ) ;
#10067 = CARTESIAN_POINT ( 'NONE',  ( -151.4692556286852891, -190.4084106276440309, 59.56931450028537967 ) ) ;
#10068 = CARTESIAN_POINT ( 'NONE',  ( 72.33162239183086228, 137.5781058455011703, 11.98183203572534872 ) ) ;
#10069 = CARTESIAN_POINT ( 'NONE',  ( -160.8964159109769696, -176.3084106276440082, 46.59394152635518793 ) ) ;
#10070 = VERTEX_POINT ( 'NONE', #6135 ) ;
#10071 = CARTESIAN_POINT ( 'NONE',  ( 47.43856463449117200, 151.7651871740939669, 32.77220824515698183 ) ) ;
#10072 = CARTESIAN_POINT ( 'NONE',  ( -55.11860757350579831, 784.8075632535900468, -3.999999999999996447 ) ) ;
#10073 = CARTESIAN_POINT ( 'NONE',  ( 46.59305225739526435, 112.5797705074273125, 36.81289934271958941 ) ) ;
#10074 = CARTESIAN_POINT ( 'NONE',  ( 53.88337135589062399, 152.3674195137575964, -9.803719146365084569 ) ) ;
#10075 = ORIENTED_EDGE ( 'NONE', *, *, #3400, .T. ) ;
#10076 = AXIS2_PLACEMENT_3D ( 'NONE', #2993, #8407, #16431 ) ;
#10077 = VERTEX_POINT ( 'NONE', #19269 ) ;
#10078 = CARTESIAN_POINT ( 'NONE',  ( 38.58424406990784661, 120.5297705074273154, 35.64915139335016647 ) ) ;
#10079 = FACE_OUTER_BOUND ( 'NONE', #15669, .T. ) ;
#10080 = CARTESIAN_POINT ( 'NONE',  ( 38.58424406990784661, 153.2651871740940237, 35.64915139335016647 ) ) ;
#10081 = CARTESIAN_POINT ( 'NONE',  ( 75.10802748102119608, 108.0013139708956800, -8.018167963582932600 ) ) ;
#10082 = CARTESIAN_POINT ( 'NONE',  ( 38.01140435219952707, 158.7844580088725763, 34.21067981925357060 ) ) ;
#10083 = DIRECTION ( 'NONE',  ( -0.000000000000000000, 1.000000000000000000, -0.000000000000000000 ) ) ;
#10084 = CARTESIAN_POINT ( 'NONE',  ( -145.2889157411863721, -175.4391397928654328, 58.16351966513671812 ) ) ;
#10085 = DIRECTION ( 'NONE',  ( 0.000000000000000000, 0.000000000000000000, 1.000000000000000000 ) ) ;
#10086 = CARTESIAN_POINT ( 'NONE',  ( -151.4692556286852891, -196.9891397928655010, 49.65701158161630957 ) ) ;
#10087 = DIRECTION ( 'NONE',  ( 0.000000000000000000, 0.000000000000000000, 1.000000000000000000 ) ) ;
#10088 = AXIS2_PLACEMENT_3D ( 'NONE', #21165, #6054, #19501 ) ;
#10089 = CARTESIAN_POINT ( 'NONE',  ( 38.01140435219952707, 98.93445800887255359, 35.83527830041809636 ) ) ;
#10090 = AXIS2_PLACEMENT_3D ( 'NONE', #14885, #9398, #7856 ) ;
#10091 = CARTESIAN_POINT ( 'NONE',  ( 43.01140435219951286, 91.12977050742732388, 38.86567161673127657 ) ) ;
#10092 = CARTESIAN_POINT ( 'NONE',  ( 34.72595348466361287, 146.8618156516888291, -3.415175568290148345 ) ) ;
#10093 = CARTESIAN_POINT ( 'NONE',  ( -143.8425227516148084, -171.0938272943107279, 44.11586579668791330 ) ) ;
#10094 = CARTESIAN_POINT ( 'NONE',  ( 39.42975644700377558, 87.41518717409401518, 36.81289934271958941 ) ) ;
#10095 = CARTESIAN_POINT ( 'NONE',  ( 173.3794444120442506, -136.9891397928655010, 67.64809332337412684 ) ) ;
#10096 = ORIENTED_EDGE ( 'NONE', *, *, #1272, .T. ) ;
#10097 = PLANE ( 'NONE',  #4848 ) ;
#10098 = CARTESIAN_POINT ( 'NONE',  ( 30.90322180743143576, 151.9278386122780375, 10.43433729856376502 ) ) ;
#10099 = CARTESIAN_POINT ( 'NONE',  ( 41.64333658814960870, 143.7797705074273154, 30.00020018409699318 ) ) ;
#10100 = CARTESIAN_POINT ( 'NONE',  ( 18.53657114080759527, 106.0614633106838909, -4.410498573173142312 ) ) ;
#10101 = AXIS2_PLACEMENT_3D ( 'NONE', #9305, #7336, #14245 ) ;
#10102 = CARTESIAN_POINT ( 'NONE',  ( 38.58424406990786082, 60.37977050742732388, 34.21067981925357060 ) ) ;
#10103 = EDGE_LOOP ( 'NONE', ( #16553, #20528, #18905, #19844, #3701, #6851 ) ) ;
#10104 = VECTOR ( 'NONE', #18592, 1000.000000000000000 ) ;
#10105 = CARTESIAN_POINT ( 'NONE',  ( 41.64333658814960870, 147.9797705074273324, 38.42115945441014446 ) ) ;
#10106 = ADVANCED_FACE ( 'NONE', ( #12865 ), #11640, .T. ) ;
#10107 = CARTESIAN_POINT ( 'NONE',  ( 42.21948215057683740, 142.3836182503285102, 39.21067981925357060 ) ) ;
#10108 = CARTESIAN_POINT ( 'NONE',  ( 44.55648932407425633, 98.81049967264873146, 29.45539723777780239 ) ) ;
#10109 = CARTESIAN_POINT ( 'NONE',  ( 45.74753988029933538, 61.16518717409398675, 37.97664729208901946 ) ) ;
#10110 =( BOUNDED_CURVE ( )  B_SPLINE_CURVE ( 2, ( #7799, #14505, #21247, #6124, #12853, #19576, #4468, #9561, #8345, #18698, #15055, #6583, #3158 ),
 .UNSPECIFIED., .F., .F. ) 
 B_SPLINE_CURVE_WITH_KNOTS ( ( 3, 2, 2, 2, 2, 2, 3 ),
 ( 0.01785714285714287350, 0.02142857142857142877, 0.02857142857142857054, 0.03571428571428571230, 0.04285714285714285754, 0.05000000000000000278, 0.05357142857142858927 ),
 .UNSPECIFIED. ) 
 CURVE ( )  GEOMETRIC_REPRESENTATION_ITEM ( )  RATIONAL_B_SPLINE_CURVE ( ( 0.9755282581475767101, 0.9755282581475768211, 1.000000000000000000, 0.9510565162951535312, 1.000000000000000000, 0.9510565162951535312, 1.000000000000000000, 0.9510565162951535312, 1.000000000000000000, 0.9510565162951535312, 1.000000000000000000, 0.9755282581475765991, 0.9755282581475767101 ) ) 
 REPRESENTATION_ITEM ( '' )  );
#10111 = CARTESIAN_POINT ( 'NONE',  ( -148.5561028927606344, -165.9938272943107336, 58.62277379824867296 ) ) ;
#10112 = CARTESIAN_POINT ( 'NONE',  ( 43.01140435219951286, 104.9604996726487371, 29.21067981925356705 ) ) ;
#10113 = CARTESIAN_POINT ( 'NONE',  ( -154.5594255724347761, -170.1630981290893203, 40.14644641866476604 ) ) ;
#10114 = DIRECTION ( 'NONE',  ( 0.000000000000000000, 1.000000000000000000, 0.000000000000000000 ) ) ;
#10115 = CARTESIAN_POINT ( 'NONE',  ( 44.55648932407425633, 142.8844580088725991, 29.45539723777780239 ) ) ;
#10116 = CARTESIAN_POINT ( 'NONE',  ( 40.27526882409969033, 126.8297705074273409, 37.97664729208901946 ) ) ;
#10117 = CARTESIAN_POINT ( 'NONE',  ( 76.78854507624612324, 113.8604396784633508, 11.78705480642107517 ) ) ;
#10118 = CARTESIAN_POINT ( 'NONE',  ( 38.01140435219952707, 140.6344580088725991, 32.58608133808903773 ) ) ;
#10119 = CIRCLE ( 'NONE', #18564, 7.500000000000007105 ) ;
#10120 = CARTESIAN_POINT ( 'NONE',  ( 44.37947211624943833, 118.0151871740940095, 38.42115945441014446 ) ) ;
#10121 = EDGE_CURVE ( 'NONE', #706, #8458, #20570, .T. ) ;
#10122 = CARTESIAN_POINT ( 'NONE',  ( 147.5268905834513475, 193.0332408774651185, 4.000000000000021316 ) ) ;
#10123 = DIRECTION ( 'NONE',  ( -0.000000000000000000, -1.000000000000000000, -0.000000000000000000 ) ) ;
#10124 = CARTESIAN_POINT ( 'NONE',  ( 75.16838608161717161, 131.4143534805274101, -0.7992312111982662337 ) ) ;
#10125 = CARTESIAN_POINT ( 'NONE',  ( 14.93692188586762803, 117.2531131035273546, 2.061388125607503952 ) ) ;
#10126 = CARTESIAN_POINT ( 'NONE',  ( -145.2889157411863437, -155.6130981290893089, 41.15050349809589392 ) ) ;
#10127 = CARTESIAN_POINT ( 'NONE',  ( 40.27526882409969744, 86.92977050742732104, 30.44471234641812174 ) ) ;
#10128 = ORIENTED_EDGE ( 'NONE', *, *, #8131, .F. ) ;
#10129 = VECTOR ( 'NONE', #2703, 1000.000000000000000 ) ;
#10130 = CARTESIAN_POINT ( 'NONE',  ( -166.4803626276155626, -116.9891397928655010, 49.65701158161629536 ) ) ;
#10131 = ORIENTED_EDGE ( 'NONE', *, *, #8453, .T. ) ;
#10132 = CARTESIAN_POINT ( 'NONE',  ( 43.01140435219951286, 74.03445800887257633, 28.95336869806222779 ) ) ;
#10133 = LINE ( 'NONE', #20377, #21811 ) ;
#10134 = VECTOR ( 'NONE', #14810, 1000.000000000000000 ) ;
#10135 = CARTESIAN_POINT ( 'NONE',  ( 47.05648932407426344, 142.9104996726487400, 37.14960608071593384 ) ) ;
#10137 = CARTESIAN_POINT ( 'NONE',  ( 17.93535261252752022, 143.0936276526352913, -10.08503035249478685 ) ) ;
#10136 = CARTESIAN_POINT ( 'NONE',  ( 38.58424406990784661, 83.96518717409399812, 32.77220824515698183 ) ) ;
#10138 = ADVANCED_FACE ( 'NONE', ( #11969 ), #5355, .T. ) ;
#10139 = CARTESIAN_POINT ( 'NONE',  ( -145.6429501568359797, -163.1084106276440195, 57.67623309621198047 ) ) ;
#10140 = CARTESIAN_POINT ( 'NONE',  ( -142.0420953463935803, -192.5438272943107449, 52.72008163687743831 ) ) ;
#10141 = CARTESIAN_POINT ( 'NONE',  ( 38.96631938032478359, 94.01049967264873430, 37.14960608071593384 ) ) ;
#10142 = DIRECTION ( 'NONE',  ( 0.3428981916074316239, -0.9393725726208708160, 0.000000000000000000 ) ) ;
#10143 = CARTESIAN_POINT ( 'NONE',  ( 42.21948215057683740, 148.3836182503284817, 39.21067981925355639 ) ) ;
#10144 = CARTESIAN_POINT ( 'NONE',  ( 41.46631938032478359, 79.31049967264873146, 38.96596240072933170 ) ) ;
#10145 = CARTESIAN_POINT ( 'NONE',  ( 38.58424406990784661, 156.2297705074273040, 32.77220824515698183 ) ) ;
#10146 = CARTESIAN_POINT ( 'NONE',  ( 66.89036333300305159, 144.4373801540182569, -2.303882249869787291 ) ) ;
#10147 = CARTESIAN_POINT ( 'NONE',  ( 47.43856463449117911, 145.7651871740939953, 32.77220824515697473 ) ) ;
#10148 = AXIS2_PLACEMENT_3D ( 'NONE', #6367, #14521, #21261 ) ;
#10149 = CARTESIAN_POINT ( 'NONE',  ( -145.6429501568359797, -159.8438272943107563, 57.67623309621198047 ) ) ;
#10150 = CARTESIAN_POINT ( 'NONE',  ( -143.8425227516148084, -177.9584106276440707, 55.19815736654470584 ) ) ;
#10151 = AXIS2_PLACEMENT_3D ( 'NONE', #11625, #21450, #16255 ) ;
#10152 = ORIENTED_EDGE ( 'NONE', *, *, #11384, .F. ) ;
#10153 = CARTESIAN_POINT ( 'NONE',  ( 38.01140435219952707, 77.63445800887255643, 32.58608133808903773 ) ) ;
#10154 = CARTESIAN_POINT ( 'NONE',  ( -157.2955611005346270, -161.6084106276440480, 41.63779006702063867 ) ) ;
#10155 = CARTESIAN_POINT ( 'NONE',  ( 41.36127970224624306, 91.67401929561202678, -0.5144393322287174053 ) ) ;
#10156 = CYLINDRICAL_SURFACE ( 'NONE', #5634, 5.000000000000004441 ) ;
#10157 = CARTESIAN_POINT ( 'NONE',  ( 47.43856463449118621, 124.6151871740940038, 34.21067981925357060 ) ) ;
#10158 = EDGE_CURVE ( 'NONE', #8286, #18069, #17817, .T. ) ;
#10159 = ORIENTED_EDGE ( 'NONE', *, *, #9191, .F. ) ;
#10160 = VERTEX_POINT ( 'NONE', #16923 ) ;
#10161 = CARTESIAN_POINT ( 'NONE',  ( -145.2889157411863437, -192.5391397928654555, 41.15050349809589392 ) ) ;
#10162 = ORIENTED_EDGE ( 'NONE', *, *, #12179, .T. ) ;
#10163 = EDGE_CURVE ( 'NONE', #20510, #4977, #18699, .T. ) ;
#10164 = CARTESIAN_POINT ( 'NONE',  ( 38.96631938032478359, 101.4844580088725792, 31.27175355779120025 ) ) ;
#10165 = CARTESIAN_POINT ( 'NONE',  ( 38.58424406990785371, 159.2297705074272756, 32.77220824515697473 ) ) ;
#10166 = CARTESIAN_POINT ( 'NONE',  ( 46.59305225739526435, 68.17977050742732104, 31.60846029578754468 ) ) ;
#10168 = CARTESIAN_POINT ( 'NONE',  ( 71.07552608251525328, 117.1481954606975791, 12.77539325861266484 ) ) ;
#10167 = CARTESIAN_POINT ( 'NONE',  ( 47.43856463449118621, 127.6151871740940038, 34.21067981925357060 ) ) ;
#10169 = EDGE_CURVE ( 'NONE', #9454, #6320, #17030, .T. ) ;
#10170 = CARTESIAN_POINT ( 'NONE',  ( 48.01140435219951996, 80.06049967264871725, 35.83527830041810347 ) ) ;
#10171 = CARTESIAN_POINT ( 'NONE',  ( 9.976645104453018220, 110.9295780357170571, 15.79146183154218619 ) ) ;
#10172 = CARTESIAN_POINT ( 'NONE',  ( 38.01140435219952707, 144.7104996726487229, 34.21067981925357060 ) ) ;
#10173 = CARTESIAN_POINT ( 'NONE',  ( -156.4692903108300186, -155.9898770414735623, 40.99677756761010272 ) ) ;
#10174 = CARTESIAN_POINT ( 'NONE',  ( 46.59305225739526435, 82.31518717409400665, 36.81289934271958941 ) ) ;
#10175 = CARTESIAN_POINT ( 'NONE',  ( 41.46631938032478359, 81.11049967264874283, 29.45539723777780239 ) ) ;
#10176 = CARTESIAN_POINT ( 'NONE',  ( 43.01140435219951286, 92.96049967264875136, 29.21067981925356705 ) ) ;
#10177 = ORIENTED_EDGE ( 'NONE', *, *, #11634, .F. ) ;
#10178 = CARTESIAN_POINT ( 'NONE',  ( 47.43856463449117200, 68.02977050742731535, 32.77220824515698183 ) ) ;
#10179 = CARTESIAN_POINT ( 'NONE',  ( -159.0959885057557983, -182.4584106276440707, 44.11586579668791330 ) ) ;
#10180 = CARTESIAN_POINT ( 'NONE',  ( 49.46632042442519861, 86.28835692931116341, 14.12497754236212977 ) ) ;
#10181 = CARTESIAN_POINT ( 'NONE',  ( -142.0420953463936087, -174.6584106276440593, 49.65701158161630957 ) ) ;
#10182 = VERTEX_POINT ( 'NONE', #3815 ) ;
#10183 = EDGE_CURVE ( 'NONE', #18126, #7422, #17242, .T. ) ;
#10184 = CARTESIAN_POINT ( 'NONE',  ( 39.42975644700377558, 149.8151871740940067, 31.60846029578754468 ) ) ;
#10185 = DIRECTION ( 'NONE',  ( -4.622506457652817044E-16, 0.000000000000000000, 1.000000000000000000 ) ) ;
#10186 = CARTESIAN_POINT ( 'NONE',  ( 43.01140435219951286, 118.1297705074273239, 38.86567161673127657 ) ) ;
#10187 = CARTESIAN_POINT ( 'NONE',  ( 75.16956835342354282, 131.6452004531123805, 5.196376467030073165 ) ) ;
#10188 = ORIENTED_EDGE ( 'NONE', *, *, #19858, .F. ) ;
#10189 = VECTOR ( 'NONE', #20433, 1000.000000000000000 ) ;
#10190 =( LENGTH_UNIT ( ) NAMED_UNIT ( * ) SI_UNIT ( .MILLI., .METRE. ) );
#10191 = ORIENTED_EDGE ( 'NONE', *, *, #14123, .T. ) ;
#10192 = CARTESIAN_POINT ( 'NONE',  ( 38.58424406990786082, 117.3797705074273097, 34.21067981925357060 ) ) ;
#10193 = DIRECTION ( 'NONE',  ( 0.000000000000000000, 0.000000000000000000, -1.000000000000000000 ) ) ;
#10194 = CARTESIAN_POINT ( 'NONE',  ( 44.37947211624943833, 155.2151871740940123, 30.00020018409699318 ) ) ;
#10195 = CARTESIAN_POINT ( 'NONE',  ( 49.23863765798637360, 86.32632880410874066, 8.129368652084252744 ) ) ;
#10196 = CARTESIAN_POINT ( 'NONE',  ( 46.10157429594899270, 82.73445800887257917, 29.95742577749336988 ) ) ;
#10197 = DIRECTION ( 'NONE',  ( 0.000000000000000000, 0.000000000000000000, 1.000000000000000000 ) ) ;
#10198 = CARTESIAN_POINT ( 'NONE',  ( -141.4692556286852891, -183.9891397928654726, 49.65701158161630957 ) ) ;
#10199 = CARTESIAN_POINT ( 'NONE',  ( 43.01140435219951286, 101.9604996726487371, 29.21067981925356705 ) ) ;
#10200 = LINE ( 'NONE', #6681, #5475 ) ;
#10201 = CARTESIAN_POINT ( 'NONE',  ( 43.80332655382220253, 91.53738109496900677, 39.21067981925355639 ) ) ;
#10202 = CARTESIAN_POINT ( 'NONE',  ( -19.70755683829218796, -31.26594044116892590, 4.000000000000021316 ) ) ;
#10203 = AXIS2_PLACEMENT_3D ( 'NONE', #15167, #15394, #4806 ) ;
#10204 = CARTESIAN_POINT ( 'NONE',  ( 41.64333658814960870, 92.77977050742731535, 30.00020018409699318 ) ) ;
#10205 = CARTESIAN_POINT ( 'NONE',  ( 17.24633477965345918, 131.3686459745448758, -4.367463884209165315 ) ) ;
#10206 = CARTESIAN_POINT ( 'NONE',  ( -151.4692556286852891, -175.1438272943107393, 59.56931450028537967 ) ) ;
#10207 = CARTESIAN_POINT ( 'NONE',  ( 40.27526882409969744, 83.66518717409398675, 30.44471234641812174 ) ) ;
#10208 = CARTESIAN_POINT ( 'NONE',  ( -148.3790856849358306, -195.3891397928654783, 40.14644641866477315 ) ) ;
#10209 = EDGE_LOOP ( 'NONE', ( #7419, #20028, #4403, #20431 ) ) ;
#10210 = EDGE_CURVE ( 'NONE', #8301, #5609, #21795, .T. ) ;
#10211 = CARTESIAN_POINT ( 'NONE',  ( 116.4417310231185780, -126.9891397928655010, 19.99999999999999645 ) ) ;
#10212 = CARTESIAN_POINT ( 'NONE',  ( 14.15704070161504369, 138.3271338521546454, 9.720138693322796897 ) ) ;
#10213 = CARTESIAN_POINT ( 'NONE',  ( 38.58424406990785371, 138.5297705074273154, 35.64915139335015937 ) ) ;
#10214 = CARTESIAN_POINT ( 'NONE',  ( 70.81223827124823345, 124.1306694702586100, -7.505929917039384058 ) ) ;
#10215 = CARTESIAN_POINT ( 'NONE',  ( 44.37947211624943833, 59.47977050742732530, 30.00020018409699318 ) ) ;
#10216 = VERTEX_POINT ( 'NONE', #3497 ) ;
#10217 = CARTESIAN_POINT ( 'NONE',  ( 38.58424406990786082, 150.3797705074273097, 34.21067981925357060 ) ) ;
#10218 = PRODUCT_DEFINITION_FORMATION_WITH_SPECIFIED_SOURCE ( 'ANY', '', #1501, .NOT_KNOWN. ) ;
#10219 = CARTESIAN_POINT ( 'NONE',  ( 47.43856463449118621, 97.87977050742732388, 34.21067981925357060 ) ) ;
#10220 = DIRECTION ( 'NONE',  ( 0.000000000000000000, 0.000000000000000000, 1.000000000000000000 ) ) ;
#10221 = CARTESIAN_POINT ( 'NONE',  ( 40.27526882409969033, 63.56518717409399954, 37.97664729208901946 ) ) ;
#10222 = DIRECTION ( 'NONE',  ( 0.000000000000000000, 0.000000000000000000, 1.000000000000000000 ) ) ;
#10223 = FACE_OUTER_BOUND ( 'NONE', #13770, .T. ) ;
#10224 = DIRECTION ( 'NONE',  ( 0.9385982292947090411, 0.3450121214752271959, -1.756657601269562932E-16 ) ) ;
#10225 = CARTESIAN_POINT ( 'NONE',  ( -145.2889157411863721, -167.6130981290893089, 41.15050349809590102 ) ) ;
#10226 = CARTESIAN_POINT ( 'NONE',  ( 38.01140435219951996, 140.6344580088725706, 32.58608133808903773 ) ) ;
#10227 = CARTESIAN_POINT ( 'NONE',  ( 46.59305225739526435, 121.5797705074273267, 36.81289934271958941 ) ) ;
#10228 = CARTESIAN_POINT ( 'NONE',  ( 23.20524185134216921, 147.9029287973646660, 23.16022673208204807 ) ) ;
#10229 = CARTESIAN_POINT ( 'NONE',  ( 43.01140435219953417, 141.5344580088726048, 39.21067981925356349 ) ) ;
#10230 = CARTESIAN_POINT ( 'NONE',  ( 41.64333658814960870, 114.7151871740940123, 38.42115945441014446 ) ) ;
#10231 = EDGE_CURVE ( 'NONE', #4183, #3570, #6704, .T. ) ;
#10232 = FACE_OUTER_BOUND ( 'NONE', #1065, .T. ) ;
#10233 = CARTESIAN_POINT ( 'NONE',  ( 69.90255027150604406, 140.9627200460241454, -1.156626220813373518 ) ) ;
#10234 = CARTESIAN_POINT ( 'NONE',  ( 60.38095089740433252, 142.1228462996803046, -2.343495028824083004 ) ) ;
#10235 = DIRECTION ( 'NONE',  ( -0.000000000000000000, 1.000000000000000000, -0.000000000000000000 ) ) ;
#10236 = CARTESIAN_POINT ( 'NONE',  ( 47.43856463449117911, 85.72977050742731819, 35.64915139335015937 ) ) ;
#10237 = EDGE_CURVE ( 'NONE', #10863, #15960, #16110, .T. ) ;
#10238 = ORIENTED_EDGE ( 'NONE', *, *, #12053, .F. ) ;
#10239 = CYLINDRICAL_SURFACE ( 'NONE', #19627, 4.999999999999997335 ) ;
#10240 =( BOUNDED_CURVE ( )  B_SPLINE_CURVE ( 2, ( #8995, #5776, #19446, #7237, #9215, #4025, #17779, #12723, #20890, #2578, #17676, #10753, #15913 ),
 .UNSPECIFIED., .F., .T. ) 
 B_SPLINE_CURVE_WITH_KNOTS ( ( 3, 2, 2, 2, 2, 2, 3 ),
 ( 0.4632352941176470784, 0.4647058823529411908, 0.4676470588235294157, 0.4705882352941176405, 0.4735294117647058654, 0.4764705882352940902, 0.4779411764705882582 ),
 .UNSPECIFIED. ) 
 CURVE ( )  GEOMETRIC_REPRESENTATION_ITEM ( )  RATIONAL_B_SPLINE_CURVE ( ( 0.9755282581475768211, 0.9755282581475768211, 1.000000000000000000, 0.9510565162951535312, 1.000000000000000000, 0.9510565162951535312, 1.000000000000000000, 0.9510565162951535312, 1.000000000000000000, 0.9510565162951535312, 1.000000000000000000, 0.9755282581475763770, 0.9755282581475768211 ) ) 
 REPRESENTATION_ITEM ( '' )  );
#10241 = CARTESIAN_POINT ( 'NONE',  ( 44.55648932407425633, 69.68445800887256780, 38.96596240072933170 ) ) ;
#10242 = CARTESIAN_POINT ( 'NONE',  ( 41.46631938032478359, 59.18445800887258201, 29.45539723777780239 ) ) ;
#10243 = AXIS2_PLACEMENT_3D ( 'NONE', #12661, #14200, #15637 ) ;
#10244 = CARTESIAN_POINT ( 'NONE',  ( 44.55648932407425633, 125.8104996726487315, 29.45539723777780239 ) ) ;
#10246 = CARTESIAN_POINT ( 'NONE',  ( 10.62509257988331335, 109.0622927966340967, -11.27555259023744405 ) ) ;
#10245 = CARTESIAN_POINT ( 'NONE',  ( 44.37947211624943833, 88.01518717409399528, 38.42115945441014446 ) ) ;
#10247 = CARTESIAN_POINT ( 'NONE',  ( -145.6429501568359797, -162.2084106276440707, 41.63779006702063867 ) ) ;
#10248 = CARTESIAN_POINT ( 'NONE',  ( -151.4692556286852891, -181.1438272943107108, 59.56931450028537256 ) ) ;
#10249 = CARTESIAN_POINT ( 'NONE',  ( 43.01140435219957681, 94.46049967264876557, 39.21067981925356349 ) ) ;
#10250 = CARTESIAN_POINT ( 'NONE',  ( -141.4692556286852891, -194.9130981290892635, 46.40781461928724383 ) ) ;
#10251 = CARTESIAN_POINT ( 'NONE',  ( 39.92123440845005433, 93.23445800887256496, 38.46393386101375711 ) ) ;
#10252 = CARTESIAN_POINT ( 'NONE',  ( -154.5594255724347761, -174.0891397928654669, 40.14644641866476604 ) ) ;
#10253 = CARTESIAN_POINT ( 'NONE',  ( 46.59305225739526435, 148.5797705074273267, 36.81289934271958941 ) ) ;
#10254 = CARTESIAN_POINT ( 'NONE',  ( -161.4692556286852891, -184.4130981290893203, 52.90620854394536821 ) ) ;
#10255 = CARTESIAN_POINT ( 'NONE',  ( 75.40436159597490473, 130.9804297329818326, 12.22031048084446248 ) ) ;
#10256 = CARTESIAN_POINT ( 'NONE',  ( 45.74753988029934249, 142.1651871740940294, 37.97664729208901235 ) ) ;
#10257 = CARTESIAN_POINT ( 'NONE',  ( -159.5594255724347761, -188.7891397928654555, 43.77915905869157598 ) ) ;
#10258 = CARTESIAN_POINT ( 'NONE',  ( -148.5561028927606344, -178.2584106276440536, 58.62277379824867296 ) ) ;
#10259 = CARTESIAN_POINT ( 'NONE',  ( 38.58424406990786082, 60.11518717409400381, 34.21067981925357060 ) ) ;
#10260 = CARTESIAN_POINT ( 'NONE',  ( -151.4692556286852891, -160.4084106276440593, 59.56931450028537967 ) ) ;
#10261 = CARTESIAN_POINT ( 'NONE',  ( 66.11232864078046134, 136.2219195394164899, -3.014685448219384334 ) ) ;
#10262 = DIRECTION ( 'NONE',  ( 1.000000000000000000, 0.000000000000000000, 0.000000000000000000 ) ) ;
#10263 = CARTESIAN_POINT ( 'NONE',  ( 39.42975644700377558, 125.8151871740940067, 31.60846029578754468 ) ) ;
#10264 = ORIENTED_EDGE ( 'NONE', *, *, #12606, .F. ) ;
#10265 = VERTEX_POINT ( 'NONE', #10652 ) ;
#10266 = CARTESIAN_POINT ( 'NONE',  ( 42.21948215057683740, 147.4575765865523067, 39.21067981925355639 ) ) ;
#10267 = EDGE_LOOP ( 'NONE', ( #15690, #2323, #5100, #9833 ) ) ;
#10268 = CARTESIAN_POINT ( 'NONE',  ( 38.96631938032478359, 104.4844580088725650, 31.27175355779120025 ) ) ;
#10269 = CARTESIAN_POINT ( 'NONE',  ( 38.58424406990785371, 153.5297705074273438, 35.64915139335015937 ) ) ;
#10270 = CARTESIAN_POINT ( 'NONE',  ( 44.82204965540746855, 59.43124467221782936, 30.14400234367972686 ) ) ;
#10272 = CARTESIAN_POINT ( 'NONE',  ( 70.22564533444385404, 112.8265553529472953, -14.05338489394683243 ) ) ;
#10271 = CARTESIAN_POINT ( 'NONE',  ( 38.58424406990784661, 120.2651871740939953, 35.64915139335016647 ) ) ;
#10273 = EDGE_CURVE ( 'NONE', #13896, #9910, #10240, .T. ) ;
#10274 = CARTESIAN_POINT ( 'NONE',  ( 44.55648932407425633, 85.61049967264872862, 38.96596240072933170 ) ) ;
#10275 = CARTESIAN_POINT ( 'NONE',  ( 48.01140435219951996, 148.1344580088725706, 35.83527830041809636 ) ) ;
#10276 = DIRECTION ( 'NONE',  ( -0.000000000000000000, 1.000000000000000000, -0.000000000000000000 ) ) ;
#10277 = DIRECTION ( 'NONE',  ( 0.000000000000000000, 0.000000000000000000, -1.000000000000000000 ) ) ;
#10278 = CARTESIAN_POINT ( 'NONE',  ( 47.43856463449118621, 79.61518717409400381, 34.21067981925357060 ) ) ;
#10279 = CARTESIAN_POINT ( 'NONE',  ( 173.3794444120442506, -34.13255853780189142, 20.00000000000001776 ) ) ;
#10280 = CARTESIAN_POINT ( 'NONE',  ( 48.01140435219951996, 127.2844580088725905, 34.21067981925357060 ) ) ;
#10281 = CARTESIAN_POINT ( 'NONE',  ( 136.0032066456581390, 182.5367998656340944, 24.47866928663567521 ) ) ;
#10282 = ORIENTED_EDGE ( 'NONE', *, *, #17923, .T. ) ;
#10283 = CARTESIAN_POINT ( 'NONE',  ( -159.0959885057557983, -188.4584106276440423, 44.11586579668791330 ) ) ;
#10284 = CARTESIAN_POINT ( 'NONE',  ( 77.24268685965694203, 120.2105100216710696, 12.57728155048203433 ) ) ;
#10285 = CARTESIAN_POINT ( 'NONE',  ( -142.0420953463936087, -177.6584106276440309, 49.65701158161630957 ) ) ;
#10286 = ORIENTED_EDGE ( 'NONE', *, *, #7877, .F. ) ;
#10287 = VECTOR ( 'NONE', #13787, 1000.000000000000000 ) ;
#10288 = CARTESIAN_POINT ( 'NONE',  ( 38.58424406990784661, 152.9651871740940123, 32.77220824515698183 ) ) ;
#10289 = AXIS2_PLACEMENT_3D ( 'NONE', #5347, #20667, #3697 ) ;
#10290 = DIRECTION ( 'NONE',  ( 0.000000000000000000, 0.000000000000000000, -1.000000000000000000 ) ) ;
#10291 = CARTESIAN_POINT ( 'NONE',  ( 38.58424406990785371, 114.2297705074273182, 32.77220824515697473 ) ) ;
#10292 = CARTESIAN_POINT ( 'NONE',  ( 57.14511974427749408, 88.72838517433189054, 6.862995836283489304 ) ) ;
#10293 = VERTEX_POINT ( 'NONE', #4339 ) ;
#10294 = CIRCLE ( 'NONE', #20143, 5.000000000000004441 ) ;
#10295 = CARTESIAN_POINT ( 'NONE',  ( 43.06284635655732274, 148.1064719378950088, -10.08176808973812655 ) ) ;
#10296 = ORIENTED_EDGE ( 'NONE', *, *, #1437, .F. ) ;
#10297 = FACE_OUTER_BOUND ( 'NONE', #18443, .T. ) ;
#10298 = CARTESIAN_POINT ( 'NONE',  ( -151.4692556286852891, -196.9891397928655010, 59.65701158161632378 ) ) ;
#10299 = CARTESIAN_POINT ( 'NONE',  ( 40.27526882409969033, 86.92977050742732104, 30.44471234641811819 ) ) ;
#10300 = CARTESIAN_POINT ( 'NONE',  ( 47.43856463449117200, 145.7651871740939953, 32.77220824515698183 ) ) ;
#10301 = CARTESIAN_POINT ( 'NONE',  ( 8.927628897234525240, 116.7075971571176751, 1.981832035706394546 ) ) ;
#10302 = STYLED_ITEM ( 'NONE', ( #16207 ), #14581 ) ;
#10303 = CARTESIAN_POINT ( 'NONE',  ( 162.0641828542163125, 116.7231784796025948, 4.000000000000021316 ) ) ;
#10304 = PLANE ( 'NONE',  #2188 ) ;
#10305 = CARTESIAN_POINT ( 'NONE',  ( -143.3790856849358306, -181.2891397928654840, 55.53486410454105027 ) ) ;
#10306 = DIRECTION ( 'NONE',  ( 0.000000000000000000, -1.000000000000000000, 0.000000000000000000 ) ) ;
#10307 = CARTESIAN_POINT ( 'NONE',  ( 54.85617982533816672, 239.2521282348021714, -3.999999999999980904 ) ) ;
#10308 = DIRECTION ( 'NONE',  ( 0.8624407588727069918, -0.5061580162706794672, 0.000000000000000000 ) ) ;
#10309 = CARTESIAN_POINT ( 'NONE',  ( 43.01140435219951286, 145.4604996726487229, 39.21067981925356349 ) ) ;
#10310 = EDGE_CURVE ( 'NONE', #20113, #3863, #11059, .T. ) ;
#10311 = CARTESIAN_POINT ( 'NONE',  ( 43.01140435219951286, 98.62977050742730967, 29.55568802177586463 ) ) ;
#10312 = CARTESIAN_POINT ( 'NONE',  ( 70.05982654948900290, 127.8813624167294023, -8.653178033719973072 ) ) ;
#10313 = CARTESIAN_POINT ( 'NONE',  ( -157.2955611005346270, -175.4438272943107506, 57.67623309621198047 ) ) ;
#10314 = EDGE_CURVE ( 'NONE', #19403, #20725, #21360, .T. ) ;
#10315 = CARTESIAN_POINT ( 'NONE',  ( 40.27526882409969744, 75.56518717409399244, 37.97664729208901235 ) ) ;
#10316 = DIRECTION ( 'NONE',  ( 0.000000000000000000, 1.000000000000000000, 0.000000000000000000 ) ) ;
#10317 = ORIENTED_EDGE ( 'NONE', *, *, #349, .F. ) ;
#10318 = DIRECTION ( 'NONE',  ( 1.915514545828640458E-16, 7.041092946335503408E-17, 1.000000000000000000 ) ) ;
#10319 = CARTESIAN_POINT ( 'NONE',  ( 43.80332655382220253, 122.8836182503284675, 29.21067981925356705 ) ) ;
#10320 = CARTESIAN_POINT ( 'NONE',  ( 69.49278103613195867, 129.3669923906968222, -0.7201859908431552659 ) ) ;
#10321 = ORIENTED_EDGE ( 'NONE', *, *, #9359, .F. ) ;
#10322 = LINE ( 'NONE', #13721, #932 ) ;
#10323 = ORIENTED_EDGE ( 'NONE', *, *, #988, .T. ) ;
#10324 = CARTESIAN_POINT ( 'NONE',  ( 46.59305225739526435, 139.5797705074273267, 36.81289934271958941 ) ) ;
#10325 = CARTESIAN_POINT ( 'NONE',  ( 45.74753988029933538, 98.32977050742731251, 30.44471234641811819 ) ) ;
#10326 = CARTESIAN_POINT ( 'NONE',  ( 43.01140435219951996, 151.4604996726487514, 39.21067981925356349 ) ) ;
#10327 = EDGE_CURVE ( 'NONE', #19429, #7439, #7559, .T. ) ;
#10328 = DIRECTION ( 'NONE',  ( -0.2803088796301151375, 0.9599098561846886035, 0.000000000000000000 ) ) ;
#10329 = LINE ( 'NONE', #5356, #6039 ) ;
#10330 = CARTESIAN_POINT ( 'NONE',  ( -151.4692556286853176, -173.3130981290892976, 39.65701158161629536 ) ) ;
#10331 = CARTESIAN_POINT ( 'NONE',  ( 43.01140435219954838, 109.4604996726487371, 39.21067981925356349 ) ) ;
#10332 = CARTESIAN_POINT ( 'NONE',  ( -145.2889157411863721, -164.6130981290893089, 41.15050349809590102 ) ) ;
#10333 = CARTESIAN_POINT ( 'NONE',  ( 147.8787791192428074, -126.9891397928655010, 0.3429884183836981459 ) ) ;
#10334 = CARTESIAN_POINT ( 'NONE',  ( 41.46631938032478359, 144.3844580088725991, 38.96596240072933170 ) ) ;
#10335 = CARTESIAN_POINT ( 'NONE',  ( 38.58424406990784661, 120.2297705074273182, 32.77220824515698183 ) ) ;
#10336 = CARTESIAN_POINT ( 'NONE',  ( 32.55111017628423298, 93.63144033427927582, -0.1575420629755377999 ) ) ;
#10337 = CARTESIAN_POINT ( 'NONE',  ( 38.96631938032478359, 140.4844580088725650, 31.27175355779120025 ) ) ;
#10338 = CARTESIAN_POINT ( 'NONE',  ( 46.59305225739526435, 103.9151871740940152, 31.60846029578754468 ) ) ;
#10339 = DIRECTION ( 'NONE',  ( -0.000000000000000000, -0.000000000000000000, 1.000000000000000000 ) ) ;
#10340 = CARTESIAN_POINT ( 'NONE',  ( 43.10205244623161036, 154.1398065127551149, -10.16071067355346358 ) ) ;
#10341 = CARTESIAN_POINT ( 'NONE',  ( 67.98812442775457043, 106.8157236907426153, -0.7957547315468347371 ) ) ;
#10342 = CARTESIAN_POINT ( 'NONE',  ( -141.4692556286852891, -186.2130981290892748, 52.90620854394536821 ) ) ;
#10343 = CARTESIAN_POINT ( 'NONE',  ( 43.01140435219951286, 83.62977050742730967, 29.55568802177586107 ) ) ;
#10344 = ORIENTED_EDGE ( 'NONE', *, *, #5185, .F. ) ;
#10345 = LINE ( 'NONE', #3728, #9748 ) ;
#10346 = CARTESIAN_POINT ( 'NONE',  ( 39.92123440845004723, 72.23445800887256496, 38.46393386101376421 ) ) ;
#10347 = CARTESIAN_POINT ( 'NONE',  ( 38.96631938032478359, 86.48445800887257917, 31.27175355779120025 ) ) ;
#10348 = ADVANCED_FACE ( 'NONE', ( #20677 ), #12616, .F. ) ;
#10349 = ADVANCED_FACE ( 'NONE', ( #9107 ), #5561, .T. ) ;
#10350 = CARTESIAN_POINT ( 'NONE',  ( 43.01140435219951286, 128.9604996726487514, 28.95336869806222779 ) ) ;
#10352 = CARTESIAN_POINT ( 'NONE',  ( 58.10477600886401461, 150.5438954262070581, -8.656458923931941385 ) ) ;
#10351 = CARTESIAN_POINT ( 'NONE',  ( 39.42975644700377558, 89.81518717409400665, 31.60846029578754468 ) ) ;
#10353 = CARTESIAN_POINT ( 'NONE',  ( -154.3824083646099439, -158.7584106276440536, 40.69124936498395328 ) ) ;
#10354 = CARTESIAN_POINT ( 'NONE',  ( -154.3824083646099439, -181.2938272943107449, 58.62277379824867296 ) ) ;
#10355 = CARTESIAN_POINT ( 'NONE',  ( -148.3790856849358306, -178.5891397928654669, 59.16757674456786020 ) ) ;
#10356 = CARTESIAN_POINT ( 'NONE',  ( -141.4692556286852891, -195.0630981290893260, 49.65701158161630957 ) ) ;
#10357 = SHAPE_REPRESENTATION_RELATIONSHIP ( 'NONE' , 'NONE' ,  #15921, #12417 ) ;
#10358 = VECTOR ( 'NONE', #5901, 1000.000000000000000 ) ;
#10359 = CARTESIAN_POINT ( 'NONE',  ( 46.10157429594899270, 68.66049967264873999, 29.95742577749336988 ) ) ;
#10360 = CARTESIAN_POINT ( 'NONE',  ( -136.6255475934131596, 760.1741454933652449, -19.99999999999996092 ) ) ;
#10361 = CARTESIAN_POINT ( 'NONE',  ( 45.74753988029933538, 151.4297705074273210, 37.97664729208901946 ) ) ;
#10362 = CARTESIAN_POINT ( 'NONE',  ( 47.43856463449117200, 104.0297705074273011, 32.77220824515698183 ) ) ;
#10363 = CARTESIAN_POINT ( 'NONE',  ( 55.94180145820917716, 151.6039095241057453, 11.26783467880839140 ) ) ;
#10364 = CARTESIAN_POINT ( 'NONE',  ( 43.01140435219951286, 135.8651871740940180, 38.86567161673127657 ) ) ;
#10365 = CARTESIAN_POINT ( 'NONE',  ( -142.0420953463935803, -156.5438272943107165, 52.72008163687743831 ) ) ;
#10366 = CARTESIAN_POINT ( 'NONE',  ( -154.3824083646099439, -178.5584106276440366, 58.62277379824867296 ) ) ;
#10367 = CARTESIAN_POINT ( 'NONE',  ( 44.37947211624943833, 59.21518717409400523, 30.00020018409699318 ) ) ;
#10368 = CIRCLE ( 'NONE', #16339, 10.00000000000000888 ) ;
#10369 = CARTESIAN_POINT ( 'NONE',  ( 57.25245068215419053, 144.3413351293631877, -3.490753295080526453 ) ) ;
#10370 = CARTESIAN_POINT ( 'NONE',  ( 38.01140435219952707, 134.9344580088725536, 35.83527830041809636 ) ) ;
#10371 = CARTESIAN_POINT ( 'NONE',  ( 46.59305225739526435, 118.3151871740940067, 36.81289934271958941 ) ) ;
#10372 =( BOUNDED_CURVE ( )  B_SPLINE_CURVE ( 2, ( #1526, #8258, #6605, #13323, #20059, #4946, #18392, #20888, #2576, #820, #16017, #2683, #3623 ),
 .UNSPECIFIED., .F., .F. ) 
 B_SPLINE_CURVE_WITH_KNOTS ( ( 3, 2, 2, 2, 2, 2, 3 ),
 ( 0.1249999999999999861, 0.1264705882352941124, 0.1294117647058823650, 0.1323529411764705899, 0.1352941176470588147, 0.1382352941176470673, 0.1397058823529411797 ),
 .UNSPECIFIED. ) 
 CURVE ( )  GEOMETRIC_REPRESENTATION_ITEM ( )  RATIONAL_B_SPLINE_CURVE ( ( 0.9755282581475765991, 0.9755282581475764880, 1.000000000000000000, 0.9510565162951535312, 1.000000000000000000, 0.9510565162951535312, 1.000000000000000000, 0.9510565162951535312, 1.000000000000000000, 0.9510565162951535312, 1.000000000000000000, 0.9755282581475768211, 0.9755282581475768211 ) ) 
 REPRESENTATION_ITEM ( '' )  );
#10373 = ORIENTED_EDGE ( 'NONE', *, *, #7348, .T. ) ;
#10374 = VERTEX_POINT ( 'NONE', #2368 ) ;
#10375 = CARTESIAN_POINT ( 'NONE',  ( -176.9699209214867892, -4.918956727831215833E-14, 30.00000000000000000 ) ) ;
#10376 = ORIENTED_EDGE ( 'NONE', *, *, #5669, .F. ) ;
#10377 = CARTESIAN_POINT ( 'NONE',  ( 41.46631938032478359, 101.1844580088725678, 29.45539723777780239 ) ) ;
#10378 = ADVANCED_FACE ( 'NONE', ( #7450 ), #19022, .F. ) ;
#10379 = CARTESIAN_POINT ( 'NONE',  ( 38.58424406990786082, 156.3797705074273097, 34.21067981925357060 ) ) ;
#10380 = CARTESIAN_POINT ( 'NONE',  ( 38.01140435219952707, 156.7104996726487514, 34.21067981925357060 ) ) ;
#10382 = CARTESIAN_POINT ( 'NONE',  ( 15.16534570839878349, 115.4582699162533288, 15.98979919289822149 ) ) ;
#10381 = CARTESIAN_POINT ( 'NONE',  ( 44.37947211624943833, 112.0151871740940095, 38.42115945441014446 ) ) ;
#10383 = CARTESIAN_POINT ( 'NONE',  ( 44.55648932407425633, 74.81049967264874567, 29.45539723777780239 ) ) ;
#10385 = CARTESIAN_POINT ( 'NONE',  ( 111.4021762516569964, 137.5714195593754710, 4.000000000000003553 ) ) ;
#10384 = DIRECTION ( 'NONE',  ( 0.000000000000000000, 0.000000000000000000, 1.000000000000000000 ) ) ;
#10386 = CARTESIAN_POINT ( 'NONE',  ( 42.21948215057684450, 124.3836182503284675, 39.21067981925355639 ) ) ;
#10387 = CARTESIAN_POINT ( 'NONE',  ( 149.5529451524149920, 187.4828467975320336, 34.00000000000001421 ) ) ;
#10388 = CARTESIAN_POINT ( 'NONE',  ( 47.43856463449117200, 82.76518717409400949, 32.77220824515698183 ) ) ;
#10389 = PRODUCT_DEFINITION_CONTEXT ( 'detailed design', #13918, 'design' ) ;
#10390 = CARTESIAN_POINT ( 'NONE',  ( 38.67287161060778544, 144.5284399170337792, 36.71770137080346785 ) ) ;
#10391 = CARTESIAN_POINT ( 'NONE',  ( -159.0959885057557983, -182.1938272943107506, 44.11586579668791330 ) ) ;
#10392 = CARTESIAN_POINT ( 'NONE',  ( 41.46631938032478359, 132.1104996726487286, 29.45539723777780239 ) ) ;
#10393 = VERTEX_POINT ( 'NONE', #15703 ) ;
#10394 = CARTESIAN_POINT ( 'NONE',  ( -157.2955611005346270, -187.7084106276440139, 57.67623309621198047 ) ) ;
#10395 = CARTESIAN_POINT ( 'NONE',  ( 77.07719282571002850, 116.5297446719512209, 12.69640610750513865 ) ) ;
#10396 = CARTESIAN_POINT ( 'NONE',  ( -151.4692556286852891, -178.4084106276440878, 59.56931450028537967 ) ) ;
#10397 = VERTEX_POINT ( 'NONE', #2258 ) ;
#10398 = CARTESIAN_POINT ( 'NONE',  ( 45.74753988029933538, 146.0651871740940067, 30.44471234641811819 ) ) ;
#10399 = CARTESIAN_POINT ( 'NONE',  ( -27.64582385433944367, -84.13255853780189852, 20.00000000000001776 ) ) ;
#10400 = CARTESIAN_POINT ( 'NONE',  ( 39.42975644700377558, 105.0797705074273125, 31.60846029578754468 ) ) ;
#10401 = CARTESIAN_POINT ( 'NONE',  ( 51.78234217841457365, 152.9971814535558963, 4.124977536042813142 ) ) ;
#10402 = ORIENTED_EDGE ( 'NONE', *, *, #16281, .T. ) ;
#10403 = CARTESIAN_POINT ( 'NONE',  ( 50.11350838007777497, 92.61696660072725251, -6.867350599827054758 ) ) ;
#10404 = VERTEX_POINT ( 'NONE', #14156 ) ;
#10405 = DIRECTION ( 'NONE',  ( -0.5010362705417046314, 0.000000000000000000, 0.8654262854811262118 ) ) ;
#10406 = CARTESIAN_POINT ( 'NONE',  ( 38.01140435219952707, 128.9344580088726104, 35.83527830041809636 ) ) ;
#10407 = VECTOR ( 'NONE', #1631, 1000.000000000000000 ) ;
#10408 = CARTESIAN_POINT ( 'NONE',  ( 43.01140435219951286, 146.3651871740939896, 29.55568802177586463 ) ) ;
#10409 = CARTESIAN_POINT ( 'NONE',  ( 40.02721236285810136, 85.80382532021769748, 0.4343372985580923329 ) ) ;
#10410 = CARTESIAN_POINT ( 'NONE',  ( 47.05648932407426344, 118.9104996726487400, 37.14960608071593384 ) ) ;
#10411 = CARTESIAN_POINT ( 'NONE',  ( -157.6495955161842062, -173.0391397928654555, 58.16351966513671812 ) ) ;
#10412 = CARTESIAN_POINT ( 'NONE',  ( 43.80332655382220253, 100.5373810949690210, 39.21067981925355639 ) ) ;
#10413 = CARTESIAN_POINT ( 'NONE',  ( -159.5594255724347761, -194.1891397928654897, 55.53486410454104316 ) ) ;
#10414 = CARTESIAN_POINT ( 'NONE',  ( 43.01140435219951286, 76.46049967264873715, 39.21067981925356349 ) ) ;
#10415 = CARTESIAN_POINT ( 'NONE',  ( -59.65946286876558702, 788.4655180356369328, -6.999999999999995559 ) ) ;
#10416 = CARTESIAN_POINT ( 'NONE',  ( 40.27526882409969033, 84.82977050742732672, 37.97664729208901946 ) ) ;
#10417 = CARTESIAN_POINT ( 'NONE',  ( 20.25093610150840107, 136.5556286039603435, -4.129180435126924564 ) ) ;
#10418 = CARTESIAN_POINT ( 'NONE',  ( -148.5561028927606344, -170.7938272943107165, 40.69124936498395328 ) ) ;
#10419 = CARTESIAN_POINT ( 'NONE',  ( 38.58424406990785371, 77.96518717409398391, 32.77220824515697473 ) ) ;
#10420 = CARTESIAN_POINT ( 'NONE',  ( -134.9004869860375777, 755.4811543468929358, -3.999999999999980904 ) ) ;
#10421 = PRODUCT_RELATED_PRODUCT_CATEGORY ( 'part', '', ( #8013 ) ) ;
#10422 = CARTESIAN_POINT ( 'NONE',  ( -159.5594255724347761, -158.1891397928654612, 55.53486410454104316 ) ) ;
#10423 = ORIENTED_EDGE ( 'NONE', *, *, #8292, .F. ) ;
#10424 = LINE ( 'NONE', #16913, #12935 ) ;
#10425 = CARTESIAN_POINT ( 'NONE',  ( 46.10157429594899270, 122.6604996726487542, 29.95742577749336988 ) ) ;
#10426 = CARTESIAN_POINT ( 'NONE',  ( 67.19681472375953035, 134.2522627023263908, 6.065787011912938453 ) ) ;
#10427 = ORIENTED_EDGE ( 'NONE', *, *, #865, .F. ) ;
#10428 = LINE ( 'NONE', #6907, #9379 ) ;
#10429 = ORIENTED_EDGE ( 'NONE', *, *, #15279, .T. ) ;
#10430 = CARTESIAN_POINT ( 'NONE',  ( 46.59305225739526435, 133.5797705074272983, 36.81289934271958941 ) ) ;
#10431 = APPLICATION_CONTEXT ( 'automotive_design' ) ;
#10432 = VECTOR ( 'NONE', #15070, 1000.000000000000000 ) ;
#10434 = EDGE_CURVE ( 'NONE', #16530, #19857, #4133, .T. ) ;
#10433 = CARTESIAN_POINT ( 'NONE',  ( 147.5268905834513475, 193.0332408774651185, 272.0939500981630204 ) ) ;
#10435 = AXIS2_PLACEMENT_3D ( 'NONE', #11779, #8051, #15088 ) ;
#10436 = CARTESIAN_POINT ( 'NONE',  ( 47.43856463449117200, 61.76518717409399528, 32.77220824515698183 ) ) ;
#10437 = LINE ( 'NONE', #17138, #18366 ) ;
#10438 = VECTOR ( 'NONE', #19524, 1000.000000000000000 ) ;
#10439 = EDGE_CURVE ( 'NONE', #735, #5296, #609, .T. ) ;
#10440 = CARTESIAN_POINT ( 'NONE',  ( 45.74753988029933538, 95.06518717409400665, 30.44471234641811819 ) ) ;
#10441 = CARTESIAN_POINT ( 'NONE',  ( -156.1828648351502409, -155.3945647575688156, 41.49286807254280518 ) ) ;
#10442 = DIRECTION ( 'NONE',  ( 0.9385982292947087080, 0.3450121214752276955, 0.000000000000000000 ) ) ;
#10443 = CARTESIAN_POINT ( 'NONE',  ( -161.4692556286853176, -166.5630981290893260, 49.65701158161630957 ) ) ;
#10444 = CARTESIAN_POINT ( 'NONE',  ( 46.10157429594899270, 145.7344580088725650, 29.95742577749337343 ) ) ;
#10445 = CARTESIAN_POINT ( 'NONE',  ( 46.59305225739526435, 124.5797705074273267, 36.81289934271958941 ) ) ;
#10446 = CARTESIAN_POINT ( 'NONE',  ( 66.97710950389229367, 104.8926460354658587, -1.705278757464820938 ) ) ;
#10447 = CARTESIAN_POINT ( 'NONE',  ( -148.3790856849358306, -184.5891397928654669, 59.16757674456786020 ) ) ;
#10448 = CARTESIAN_POINT ( 'NONE',  ( 41.64333658814960870, 108.7151871740940123, 38.42115945441014446 ) ) ;
#10449 = CYLINDRICAL_SURFACE ( 'NONE', #9435, 4.999999999999997335 ) ;
#10450 = CARTESIAN_POINT ( 'NONE',  ( 71.14040157825178312, 139.4183699182763974, -9.089337262093875935 ) ) ;
#10451 = VECTOR ( 'NONE', #5252, 1000.000000000000000 ) ;
#10452 = CARTESIAN_POINT ( 'NONE',  ( 15.66613903973849986, 126.7949701480144711, 9.441967288829692606 ) ) ;
#10453 = CARTESIAN_POINT ( 'NONE',  ( -145.2889157411863437, -185.6130981290893089, 41.15050349809589392 ) ) ;
#10454 = ADVANCED_FACE ( 'NONE', ( #5673 ), #19130, .F. ) ;
#10455 = CARTESIAN_POINT ( 'NONE',  ( 47.43856463449117911, 88.72977050742730398, 35.64915139335015937 ) ) ;
#10456 = CIRCLE ( 'NONE', #16062, 24.99999999999998934 ) ;
#10457 = EDGE_LOOP ( 'NONE', ( #21244, #1899, #10052, #10021 ) ) ;
#10458 = DIRECTION ( 'NONE',  ( 0.000000000000000000, 1.000000000000000000, 0.000000000000000000 ) ) ;
#10459 = CARTESIAN_POINT ( 'NONE',  ( 38.96631938032478359, 77.48445800887257917, 31.27175355779120025 ) ) ;
#10460 = CARTESIAN_POINT ( 'NONE',  ( -148.3790856849358306, -164.4630981290893317, 40.14644641866477315 ) ) ;
#10461 = CARTESIAN_POINT ( 'NONE',  ( 48.01140435219951996, 125.3604996726487286, 32.58608133808903773 ) ) ;
#10463 = CARTESIAN_POINT ( 'NONE',  ( 54.72474920843421131, 151.9887481548900325, -8.775581469602226292 ) ) ;
#10462 = CARTESIAN_POINT ( 'NONE',  ( 38.58424406990784661, 84.26518717409399528, 35.64915139335016647 ) ) ;
#10464 = VECTOR ( 'NONE', #8099, 1000.000000000000114 ) ;
#10465 = CARTESIAN_POINT ( 'NONE',  ( -160.8964159109769696, -161.0084106276440252, 52.72008163687743121 ) ) ;
#10466 = CARTESIAN_POINT ( 'NONE',  ( -151.4692556286852891, -185.6438272943107393, 39.74470866294723947 ) ) ;
#10467 = CARTESIAN_POINT ( 'NONE',  ( 43.01140435219951996, 10.71049967264875491, 34.21067981925357060 ) ) ;
#10468 = CARTESIAN_POINT ( 'NONE',  ( -159.5594255724347761, -193.2630981290893146, 55.53486410454104316 ) ) ;
#10469 = CARTESIAN_POINT ( 'NONE',  ( 43.01140435219951996, 10.71049967264875491, 34.21067981925357060 ) ) ;
#10470 = CARTESIAN_POINT ( 'NONE',  ( -151.4692556286852607, -172.7391397928654726, 59.65701158161632378 ) ) ;
#10471 = CARTESIAN_POINT ( 'NONE',  ( 44.37947211624943833, 149.4797705074273324, 30.00020018409699318 ) ) ;
#10472 = CARTESIAN_POINT ( 'NONE',  ( 41.64333658814960870, 101.7797705074273154, 30.00020018409699318 ) ) ;
#10473 = EDGE_CURVE ( 'NONE', #17856, #16317, #6940, .T. ) ;
#10474 = CARTESIAN_POINT ( 'NONE',  ( 49.46632042442519861, 86.28835692931116341, 14.12497754236212977 ) ) ;
#10475 = CARTESIAN_POINT ( 'NONE',  ( 40.27526882409969744, 137.6651871740940010, 30.44471234641812174 ) ) ;
#10476 = CARTESIAN_POINT ( 'NONE',  ( -153.0531000319306543, -187.8160212151857422, 59.65701158161632378 ) ) ;
#10477 = CARTESIAN_POINT ( 'NONE',  ( -145.6429501568359797, -168.2084106276440139, 41.63779006702063867 ) ) ;
#10478 = DIRECTION ( 'NONE',  ( 0.000000000000000000, -0.000000000000000000, 1.000000000000000000 ) ) ;
#10479 = CARTESIAN_POINT ( 'NONE',  ( 50.34320592624661828, 92.59351467088818310, -0.8717445255428065698 ) ) ;
#10480 = CARTESIAN_POINT ( 'NONE',  ( 40.27526882409969033, 111.5651871740939782, 37.97664729208901946 ) ) ;
#10481 = EDGE_CURVE ( 'NONE', #6227, #13430, #4781, .T. ) ;
#10482 = ORIENTED_EDGE ( 'NONE', *, *, #21194, .F. ) ;
#10483 = CARTESIAN_POINT ( 'NONE',  ( -161.4692556286853176, -179.4891397928654726, 49.65701158161630957 ) ) ;
#10484 = ORIENTED_EDGE ( 'NONE', *, *, #13823, .F. ) ;
#10485 = CARTESIAN_POINT ( 'NONE',  ( 43.01140435219951286, 101.0344580088725763, 28.95336869806222779 ) ) ;
#10486 = CARTESIAN_POINT ( 'NONE',  ( 45.74753988029934249, 148.4297705074273210, 37.97664729208901235 ) ) ;
#10487 = CARTESIAN_POINT ( 'NONE',  ( 43.01140435219951286, 154.4604996726487798, 39.46799094044489209 ) ) ;
#10489 = CARTESIAN_POINT ( 'NONE',  ( 69.68673170630326297, 129.0522134326295145, 12.29911014595921692 ) ) ;
#10488 = CARTESIAN_POINT ( 'NONE',  ( 39.42975644700377558, 120.4151871740940010, 36.81289934271958941 ) ) ;
#10490 = VECTOR ( 'NONE', #7144, 1000.000000000000000 ) ;
#10491 = CARTESIAN_POINT ( 'NONE',  ( 47.05648932407426344, 70.91049967264873999, 37.14960608071593384 ) ) ;
#10492 = CARTESIAN_POINT ( 'NONE',  ( 44.31111858724877095, 144.8753732970614863, 29.37128083581765381 ) ) ;
#10493 = CARTESIAN_POINT ( 'NONE',  ( -151.4692556286853176, -173.3130981290892976, 39.65701158161629536 ) ) ;
#10494 = CARTESIAN_POINT ( 'NONE',  ( 43.33818195800462547, 94.90707761860556957, 29.21067981925357060 ) ) ;
#10495 = CARTESIAN_POINT ( 'NONE',  ( 45.74753988029933538, 83.06518717409400665, 30.44471234641811819 ) ) ;
#10496 = CARTESIAN_POINT ( 'NONE',  ( 45.22505347682923116, 59.38050100342834270, 30.37668637662395099 ) ) ;
#10497 = VECTOR ( 'NONE', #20180, 1000.000000000000000 ) ;
#10498 = CARTESIAN_POINT ( 'NONE',  ( -160.8964159109769696, -185.0438272943107165, 46.59394152635518793 ) ) ;
#10499 = CARTESIAN_POINT ( 'NONE',  ( 111.4021762516569964, 137.5714195593754710, -19.99999999999997868 ) ) ;
#10500 = EDGE_LOOP ( 'NONE', ( #17133, #21309, #10402, #3225, #14226, #21537, #4686, #5528 ) ) ;
#10501 =( BOUNDED_CURVE ( )  B_SPLINE_CURVE ( 2, ( #13716, #5346, #12061, #20880, #491, #14037, #2462, #20772, #9202, #7549, #812, #15901, #5663 ),
 .UNSPECIFIED., .F., .F. ) 
 B_SPLINE_CURVE_WITH_KNOTS ( ( 3, 2, 2, 2, 2, 2, 3 ),
 ( 0.4464285714285714524, 0.4500000000000000111, 0.4571428571428571286, 0.4642857142857143016, 0.4714285714285714191, 0.4785714285714285920, 0.4821428571428571508 ),
 .UNSPECIFIED. ) 
 CURVE ( )  GEOMETRIC_REPRESENTATION_ITEM ( )  RATIONAL_B_SPLINE_CURVE ( ( 0.9755282581475768211, 0.9755282581475769321, 1.000000000000000000, 0.9510565162951535312, 1.000000000000000000, 0.9510565162951535312, 1.000000000000000000, 0.9510565162951535312, 1.000000000000000000, 0.9510565162951535312, 1.000000000000000000, 0.9755282581475768211, 0.9755282581475768211 ) ) 
 REPRESENTATION_ITEM ( '' )  );
#10502 = CARTESIAN_POINT ( 'NONE',  ( -148.5561028927606344, -180.0584106276440366, 40.69124936498395328 ) ) ;
#10503 = CARTESIAN_POINT ( 'NONE',  ( 60.35187701982888342, 149.5179833730722407, -3.570052342179399485 ) ) ;
#10504 = EDGE_CURVE ( 'NONE', #8850, #9830, #3376, .T. ) ;
#10505 = VERTEX_POINT ( 'NONE', #14913 ) ;
#10506 = CARTESIAN_POINT ( 'NONE',  ( 38.58424406990784661, 147.2651871740939669, 35.64915139335016647 ) ) ;
#10507 = CARTESIAN_POINT ( 'NONE',  ( -55.11860757350579831, 784.8075632535900468, -19.99999999999997868 ) ) ;
#10508 = CARTESIAN_POINT ( 'NONE',  ( 46.59305225739526435, 100.5797705074273267, 36.81289934271958941 ) ) ;
#10509 = CARTESIAN_POINT ( 'NONE',  ( 66.76198117565915879, 95.25264312590786631, -0.5179092472497510702 ) ) ;
#10510 = ORIENTED_EDGE ( 'NONE', *, *, #17917, .T. ) ;
#10511 = CARTESIAN_POINT ( 'NONE',  ( 14.93692188586762803, 117.2531131035273546, 2.061388125607503952 ) ) ;
#10512 = ORIENTED_EDGE ( 'NONE', *, *, #9090, .T. ) ;
#10513 = CARTESIAN_POINT ( 'NONE',  ( 45.74753988029933538, 113.3297705074273125, 30.44471234641811819 ) ) ;
#10514 = CARTESIAN_POINT ( 'NONE',  ( 173.3794444120442506, -126.9891397928655010, 19.99999999999999645 ) ) ;
#10515 = MECHANICAL_DESIGN_GEOMETRIC_PRESENTATION_REPRESENTATION (  '', ( #21413 ), #20361 ) ;
#10516 = LINE ( 'NONE', #17646, #19575 ) ;
#10517 = CARTESIAN_POINT ( 'NONE',  ( 38.58424406990784661, 146.9651871740940123, 32.77220824515698183 ) ) ;
#10518 = EDGE_CURVE ( 'NONE', #17794, #16883, #18001, .T. ) ;
#10519 = CARTESIAN_POINT ( 'NONE',  ( 38.01140435219952707, 99.71049967264875136, 34.21067981925357060 ) ) ;
#10520 = CARTESIAN_POINT ( 'NONE',  ( 8.779377865064803999, 119.6051361893432130, -4.922546661887801100 ) ) ;
#10521 = CARTESIAN_POINT ( 'NONE',  ( 136.0032066456581674, 182.5367998656340944, 18.98992973508700643 ) ) ;
#10522 = CARTESIAN_POINT ( 'NONE',  ( -154.5594255724347761, -169.8891397928654499, 59.16757674456785310 ) ) ;
#10523 = CARTESIAN_POINT ( 'NONE',  ( -151.4692556286852891, -180.8130981290893260, 59.65701158161631668 ) ) ;
#10524 = CARTESIAN_POINT ( 'NONE',  ( 15.75986397150585816, 99.18880659646561071, -5.637120474378671808 ) ) ;
#10525 = CARTESIAN_POINT ( 'NONE',  ( 116.4417310231185780, -126.9891397928655010, 19.99999999999999645 ) ) ;
#10526 = CARTESIAN_POINT ( 'NONE',  ( 38.58424406990784661, 87.52977050742730114, 35.64915139335016647 ) ) ;
#10527 = CARTESIAN_POINT ( 'NONE',  ( -160.8964159109769696, -176.0438272943107165, 46.59394152635518793 ) ) ;
#10528 = CARTESIAN_POINT ( 'NONE',  ( 43.01140435219951286, 80.36518717409398960, 29.55568802177586107 ) ) ;
#10529 = DIRECTION ( 'NONE',  ( 0.000000000000000000, 0.000000000000000000, 1.000000000000000000 ) ) ;
#10530 = CARTESIAN_POINT ( 'NONE',  ( 141.4773229304660447, 84.89323405393692212, 4.000000000000021316 ) ) ;
#10531 = ORIENTED_EDGE ( 'NONE', *, *, #1934, .T. ) ;
#10532 = CARTESIAN_POINT ( 'NONE',  ( 48.01140435219951996, 85.28445800887257633, 34.21067981925357060 ) ) ;
#10533 = CARTESIAN_POINT ( 'NONE',  ( 43.01140435219951286, 121.4604996726487371, 39.21067981925356349 ) ) ;
#10534 = CARTESIAN_POINT ( 'NONE',  ( 45.74753988029934249, 137.3297705074272983, 30.44471234641812174 ) ) ;
#10535 = CARTESIAN_POINT ( 'NONE',  ( 74.63589561985200760, 132.8035080205385157, -14.84689682711585768 ) ) ;
#10536 = ORIENTED_EDGE ( 'NONE', *, *, #15749, .F. ) ;
#10537 = DIRECTION ( 'NONE',  ( 0.000000000000000000, -0.000000000000000000, 1.000000000000000000 ) ) ;
#10538 = VERTEX_POINT ( 'NONE', #3022 ) ;
#10539 = CARTESIAN_POINT ( 'NONE',  ( 47.43856463449117200, 133.7297705074273324, 35.64915139335016647 ) ) ;
#10540 = CARTESIAN_POINT ( 'NONE',  ( -141.4692556286852891, -181.1391397928654783, 52.90620854394536821 ) ) ;
#10541 = VECTOR ( 'NONE', #21461, 1000.000000000000000 ) ;
#10542 = CARTESIAN_POINT ( 'NONE',  ( 44.37947211624943833, 62.21518717409399102, 30.00020018409699318 ) ) ;
#10543 = CARTESIAN_POINT ( 'NONE',  ( -151.4692556286852607, -168.8130981290893260, 59.65701158161632378 ) ) ;
#10544 = CARTESIAN_POINT ( 'NONE',  ( -149.8854112254399524, -191.3899795514095956, 39.65701158161630957 ) ) ;
#10545 = CARTESIAN_POINT ( 'NONE',  ( 45.74753988029933538, 98.06518717409397823, 30.44471234641811819 ) ) ;
#10546 = CYLINDRICAL_SURFACE ( 'NONE', #8295, 10.00000000000000888 ) ;
#10547 = CARTESIAN_POINT ( 'NONE',  ( -159.5594255724347761, -172.2630981290892862, 55.53486410454104316 ) ) ;
#10548 =( LENGTH_UNIT ( ) NAMED_UNIT ( * ) SI_UNIT ( .MILLI., .METRE. ) );
#10549 = CARTESIAN_POINT ( 'NONE',  ( 39.92123440845004723, 143.3344580088725877, 29.95742577749337343 ) ) ;
#10550 = CARTESIAN_POINT ( 'NONE',  ( 39.42975644700377558, 117.0797705074273267, 31.60846029578754468 ) ) ;
#10551 = CARTESIAN_POINT ( 'NONE',  ( 28.23826046203858908, 88.93502212982269839, 20.83457506318435648 ) ) ;
#10552 = CARTESIAN_POINT ( 'NONE',  ( -148.3790856849358306, -183.3891397928654783, 40.14644641866477315 ) ) ;
#10553 = CARTESIAN_POINT ( 'NONE',  ( 47.43856463449118621, 109.6151871740940038, 34.21067981925357060 ) ) ;
#10554 = VERTEX_POINT ( 'NONE', #21663 ) ;
#10555 = CARTESIAN_POINT ( 'NONE',  ( 43.01140435219951286, 88.46049967264873715, 39.21067981925356349 ) ) ;
#10556 = CARTESIAN_POINT ( 'NONE',  ( 8.922311181598237440, 122.0085103898528018, 10.15299703236346573 ) ) ;
#10557 = EDGE_CURVE ( 'NONE', #18667, #7658, #11176, .T. ) ;
#10558 = CARTESIAN_POINT ( 'NONE',  ( 19.85370653151704090, 103.8158566922722486, 8.489678972899794118 ) ) ;
#10559 = CARTESIAN_POINT ( 'NONE',  ( -151.4692556286852607, -169.7391397928654442, 59.65701158161632378 ) ) ;
#10560 =( REPRESENTATION_RELATIONSHIP ('NONE','NONE', #6933, #8609 ) REPRESENTATION_RELATIONSHIP_WITH_TRANSFORMATION ( #4905 )SHAPE_REPRESENTATION_RELATIONSHIP( ) );
#10561 = STYLED_ITEM ( 'NONE', ( #13055 ), #21708 ) ;
#10562 = CARTESIAN_POINT ( 'NONE',  ( 39.42975644700377558, 87.07977050742732672, 31.60846029578754468 ) ) ;
#10563 = VERTEX_POINT ( 'NONE', #16455 ) ;
#10564 = CARTESIAN_POINT ( 'NONE',  ( 39.92123440845004723, 71.33445800887258770, 29.95742577749337343 ) ) ;
#10565 = DIRECTION ( 'NONE',  ( -1.140132994654635861E-16, -0.000000000000000000, -1.000000000000000000 ) ) ;
#10566 = CARTESIAN_POINT ( 'NONE',  ( 38.96631938032478359, 133.0104996726487343, 37.14960608071593384 ) ) ;
#10568 = CARTESIAN_POINT ( 'NONE',  ( 17.98086284713512129, 132.6641746743869135, 10.68742175872072409 ) ) ;
#10567 = CARTESIAN_POINT ( 'NONE',  ( 39.42975644700377558, 87.41518717409401518, 36.81289934271958941 ) ) ;
#10569 = CARTESIAN_POINT ( 'NONE',  ( -148.5561028927606344, -160.2584106276440536, 58.62277379824867296 ) ) ;
#10570 = CARTESIAN_POINT ( 'NONE',  ( -151.4692556286852891, -182.6438272943106824, 39.74470866294723947 ) ) ;
#10571 = CARTESIAN_POINT ( 'NONE',  ( 43.01140435219951286, 92.96049967264875136, 29.21067981925356705 ) ) ;
#10572 = DIRECTION ( 'NONE',  ( 0.000000000000000000, 1.000000000000000000, 0.000000000000000000 ) ) ;
#10573 = FACE_BOUND ( 'NONE', #5055, .T. ) ;
#10574 = CARTESIAN_POINT ( 'NONE',  ( -81.61981105773979550, 604.5992151483073940, -23.16745088979876499 ) ) ;
#10575 = CARTESIAN_POINT ( 'NONE',  ( 47.43856463449117200, 140.0297705074273438, 32.77220824515698183 ) ) ;
#10576 = CARTESIAN_POINT ( 'NONE',  ( 47.43856463449117200, 101.0297705074273011, 32.77220824515698183 ) ) ;
#10577 = CARTESIAN_POINT ( 'NONE',  ( 39.42975644700377558, 134.8151871740940067, 31.60846029578754468 ) ) ;
#10578 = CARTESIAN_POINT ( 'NONE',  ( -161.4692556286853176, -188.4891397928654726, 49.65701158161630957 ) ) ;
#10579 = CARTESIAN_POINT ( 'NONE',  ( -145.6429501568359797, -163.1084106276440195, 57.67623309621197336 ) ) ;
#10580 = CARTESIAN_POINT ( 'NONE',  ( 38.58424406990784661, 63.22977050742731109, 32.77220824515698183 ) ) ;
#10581 = CARTESIAN_POINT ( 'NONE',  ( 43.01140435219951286, 136.4604996726487514, 39.21067981925356349 ) ) ;
#10582 = ADVANCED_FACE ( 'NONE', ( #17888 ), #14806, .F. ) ;
#10583 = CARTESIAN_POINT ( 'NONE',  ( 18.61283035262889385, 105.6058852300018032, 7.580709131559767222 ) ) ;
#10584 = DIRECTION ( 'NONE',  ( -0.000000000000000000, -0.000000000000000000, -1.000000000000000000 ) ) ;
#10585 = CARTESIAN_POINT ( 'NONE',  ( 39.42975644700377558, 117.4151871740940010, 36.81289934271958941 ) ) ;
#10586 = EDGE_LOOP ( 'NONE', ( #3181, #8749, #222, #18771 ) ) ;
#10587 = CARTESIAN_POINT ( 'NONE',  ( -161.4692556286852891, -160.4130981290893203, 52.90620854394536821 ) ) ;
#10588 = ORIENTED_EDGE ( 'NONE', *, *, #9100, .T. ) ;
#10589 = CARTESIAN_POINT ( 'NONE',  ( 41.46631938032478359, 99.38445800887258486, 38.96596240072933170 ) ) ;
#10590 = ADVANCED_BREP_SHAPE_REPRESENTATION ( '', ( #7141, #12657 ), #17239 ) ;
#10591 = CARTESIAN_POINT ( 'NONE',  ( 48.01140435219951996, 158.2104996726487514, 34.21067981925357060 ) ) ;
#10593 = CARTESIAN_POINT ( 'NONE',  ( 56.80456144658707274, 95.31062238922963559, 13.84685026556700116 ) ) ;
#10592 = CARTESIAN_POINT ( 'NONE',  ( 46.59305225739526435, 118.9151871740940010, 31.60846029578754468 ) ) ;
#10594 = CARTESIAN_POINT ( 'NONE',  ( 46.10157429594899270, 67.76049967264872009, 38.46393386101376421 ) ) ;
#10596 = CARTESIAN_POINT ( 'NONE',  ( 43.01140435219951996, 10.71049967264875491, 34.21067981925357060 ) ) ;
#10595 = CARTESIAN_POINT ( 'NONE',  ( 38.01140435219952707, 107.7844580088725763, 34.21067981925357060 ) ) ;
#10597 = EDGE_CURVE ( 'NONE', #10835, #6960, #21328, .T. ) ;
#10598 = EDGE_CURVE ( 'NONE', #11010, #8663, #12299, .T. ) ;
#10599 = LINE ( 'NONE', #2535, #19864 ) ;
#10600 = CARTESIAN_POINT ( 'NONE',  ( 148.6725454929228079, -61.68114226949890622, 20.00000000000001776 ) ) ;
#10601 = CARTESIAN_POINT ( 'NONE',  ( 47.43856463449117200, 79.46518717409399812, 35.64915139335016647 ) ) ;
#10602 = DIRECTION ( 'NONE',  ( -0.000000000000000000, -0.000000000000000000, -1.000000000000000000 ) ) ;
#10603 = CARTESIAN_POINT ( 'NONE',  ( -143.8425227516148084, -183.0938272943107279, 44.11586579668791330 ) ) ;
#10604 = CARTESIAN_POINT ( 'NONE',  ( -160.8964159109769696, -194.0084106276440252, 52.72008163687743121 ) ) ;
#10605 = ORIENTED_EDGE ( 'NONE', *, *, #325, .T. ) ;
#10606 = CARTESIAN_POINT ( 'NONE',  ( -157.2955611005346270, -176.6084106276440195, 41.63779006702063867 ) ) ;
#10607 = CARTESIAN_POINT ( 'NONE',  ( 11.87357267856223864, 134.3244722033052767, 8.572888645784400907 ) ) ;
#10608 = ORIENTED_EDGE ( 'NONE', *, *, #4767, .T. ) ;
#10609 = CARTESIAN_POINT ( 'NONE',  ( 41.64333658814960870, 147.7151871740940123, 38.42115945441014446 ) ) ;
#10610 = DIRECTION ( 'NONE',  ( -0.4999999999999996114, 0.000000000000000000, -0.8660254037844388186 ) ) ;
#10611 = CARTESIAN_POINT ( 'NONE',  ( 47.43856463449117911, 103.7297705074273182, 35.64915139335015937 ) ) ;
#10612 = CARTESIAN_POINT ( 'NONE',  ( 11.67247064774405452, 106.1322524520788875, 1.624861436118421043 ) ) ;
#10613 = ORIENTED_EDGE ( 'NONE', *, *, #364, .T. ) ;
#10614 = CARTESIAN_POINT ( 'NONE',  ( 54.67410106651116308, 94.23276814491528341, 6.942135068398441078 ) ) ;
#10615 = ORIENTED_EDGE ( 'NONE', *, *, #7850, .F. ) ;
#10616 = CARTESIAN_POINT ( 'NONE',  ( 39.42975644700377558, 111.0797705074273125, 31.60846029578754468 ) ) ;
#10617 = DIRECTION ( 'NONE',  ( 0.000000000000000000, -0.000000000000000000, -1.000000000000000000 ) ) ;
#10618 = DIRECTION ( 'NONE',  ( 1.000000000000000000, 0.000000000000000000, 0.000000000000000000 ) ) ;
#10619 = CARTESIAN_POINT ( 'NONE',  ( 46.59305225739526435, 83.17977050742732104, 31.60846029578754468 ) ) ;
#10620 = CARTESIAN_POINT ( 'NONE',  ( 39.42975644700377558, 146.8151871740940067, 31.60846029578754468 ) ) ;
#10621 = CARTESIAN_POINT ( 'NONE',  ( 38.96631938032478359, 97.01049967264874851, 37.14960608071593384 ) ) ;
#10622 = CARTESIAN_POINT ( 'NONE',  ( 33.56091001181424360, 87.00402361476987778, -6.351118090676544981 ) ) ;
#10623 = EDGE_CURVE ( 'NONE', #16314, #17801, #18111, .T. ) ;
#10624 = CARTESIAN_POINT ( 'NONE',  ( 38.01140435219952707, 60.56049967264873146, 32.58608133808903773 ) ) ;
#10625 = CARTESIAN_POINT ( 'NONE',  ( -159.5594255724347761, -167.7891397928654840, 43.77915905869157598 ) ) ;
#10626 =( BOUNDED_CURVE ( )  B_SPLINE_CURVE ( 2, ( #19871, #2781, #14678, #4758, #16327, #4538, #1236, #14457, #2665, #16117, #12923, #9521, #18205 ),
 .UNSPECIFIED., .F., .F. ) 
 B_SPLINE_CURVE_WITH_KNOTS ( ( 3, 2, 2, 2, 2, 2, 3 ),
 ( 0.5073529411764705621, 0.5088235294117646745, 0.5117647058823528994, 0.5147058823529411242, 0.5176470588235294601, 0.5205882352941176849, 0.5220588235294117974 ),
 .UNSPECIFIED. ) 
 CURVE ( )  GEOMETRIC_REPRESENTATION_ITEM ( )  RATIONAL_B_SPLINE_CURVE ( ( 0.9755282581475768211, 0.9755282581475768211, 1.000000000000000000, 0.9510565162951535312, 1.000000000000000000, 0.9510565162951535312, 1.000000000000000000, 0.9510565162951535312, 1.000000000000000000, 0.9510565162951535312, 1.000000000000000000, 0.9755282581475768211, 0.9755282581475768211 ) ) 
 REPRESENTATION_ITEM ( '' )  );
#10627 = DIRECTION ( 'NONE',  ( 0.000000000000000000, 1.000000000000000000, 0.000000000000000000 ) ) ;
#10628 = UNCERTAINTY_MEASURE_WITH_UNIT (LENGTH_MEASURE( 1.000000000000000082E-05 ), #12225, 'distance_accuracy_value', 'NONE');
#10629 = FACE_OUTER_BOUND ( 'NONE', #4049, .T. ) ;
#10630 = VECTOR ( 'NONE', #15687, 1000.000000000000000 ) ;
#10631 = CARTESIAN_POINT ( 'NONE',  ( 116.4417310231185780, -126.9891397928655010, 0.3429884183836981459 ) ) ;
#10632 = VECTOR ( 'NONE', #14038, 1000.000000000000000 ) ;
#10633 = VERTEX_POINT ( 'NONE', #11616 ) ;
#10634 = CARTESIAN_POINT ( 'NONE',  ( 38.58424406990786082, 81.37977050742730967, 34.21067981925357060 ) ) ;
#10635 = CARTESIAN_POINT ( 'NONE',  ( 47.43856463449117911, 76.46518717409401233, 35.64915139335015937 ) ) ;
#10636 = CARTESIAN_POINT ( 'NONE',  ( 43.10205244623161036, 154.1398065127551149, -10.16071067355346358 ) ) ;
#10637 = CARTESIAN_POINT ( 'NONE',  ( -143.8425227516148084, -195.3584106276440480, 44.11586579668791330 ) ) ;
#10638 = ORIENTED_EDGE ( 'NONE', *, *, #20781, .T. ) ;
#10639 = DIRECTION ( 'NONE',  ( 0.9385982292947087080, 0.3450121214752278620, -2.040824802394967678E-16 ) ) ;
#10640 = FACE_OUTER_BOUND ( 'NONE', #8933, .T. ) ;
#10641 = CARTESIAN_POINT ( 'NONE',  ( 38.58424406990785371, 129.2297705074273040, 32.77220824515697473 ) ) ;
#10642 = CARTESIAN_POINT ( 'NONE',  ( 50.95956618318000864, 146.8798181090472212, 5.232242258870305918 ) ) ;
#10643 = ORIENTED_EDGE ( 'NONE', *, *, #1697, .F. ) ;
#10644 = CARTESIAN_POINT ( 'NONE',  ( -133.8097529055291943, 761.2091818577913500, -6.999999999999982236 ) ) ;
#10645 = ORIENTED_EDGE ( 'NONE', *, *, #21469, .T. ) ;
#10646 = CARTESIAN_POINT ( 'NONE',  ( 38.58424406990786082, 138.3797705074273381, 34.21067981925357060 ) ) ;
#10647 = VECTOR ( 'NONE', #6260, 1000.000000000000000 ) ;
#10648 = CIRCLE ( 'NONE', #13460, 16.96660865288809816 ) ;
#10649 = CARTESIAN_POINT ( 'NONE',  ( 38.58424406990784661, 93.52977050742731535, 35.64915139335016647 ) ) ;
#10650 = DIRECTION ( 'NONE',  ( -0.000000000000000000, -0.000000000000000000, -1.000000000000000000 ) ) ;
#10651 = VECTOR ( 'NONE', #5229, 1000.000000000000000 ) ;
#10652 = CARTESIAN_POINT ( 'NONE',  ( 156.5268905834513475, 193.0332408774651185, -50.99999999999998579 ) ) ;
#10653 = CARTESIAN_POINT ( 'NONE',  ( -151.4692556286852891, -192.8130981290892692, 59.65701158161632378 ) ) ;
#10654 = CARTESIAN_POINT ( 'NONE',  ( 45.74753988029933538, 94.16518717409400097, 37.97664729208901946 ) ) ;
#10655 = CARTESIAN_POINT ( 'NONE',  ( 42.21948215057683740, 153.0373810949689926, 29.21067981925357415 ) ) ;
#10656 = DIRECTION ( 'NONE',  ( 0.4874675571821264763, 0.8731411001063288380, -0.000000000000000000 ) ) ;
#10657 = CARTESIAN_POINT ( 'NONE',  ( -151.4692556286852891, -158.3130981290892976, 39.14238933923362396 ) ) ;
#10658 = DIRECTION ( 'NONE',  ( 1.000000000000000000, 0.000000000000000000, 0.000000000000000000 ) ) ;
#10659 = CARTESIAN_POINT ( 'NONE',  ( 44.55648932407425633, 133.8844580088725706, 29.45539723777780239 ) ) ;
#10660 = CARTESIAN_POINT ( 'NONE',  ( 38.58424406990786082, 117.3797705074273097, 34.21067981925357060 ) ) ;
#10661 = CARTESIAN_POINT ( 'NONE',  ( 42.84661501159713026, 148.1872198635363134, -4.086158671962061284 ) ) ;
#10662 = CARTESIAN_POINT ( 'NONE',  ( -148.5561028927606344, -192.9938272943107336, 58.62277379824867296 ) ) ;
#10663 = CARTESIAN_POINT ( 'NONE',  ( 47.43856463449118621, 106.6151871740940038, 34.21067981925357060 ) ) ;
#10664 = ORIENTED_EDGE ( 'NONE', *, *, #3564, .F. ) ;
#10665 = DIRECTION ( 'NONE',  ( 0.000000000000000000, 0.000000000000000000, 1.000000000000000000 ) ) ;
#10666 = CARTESIAN_POINT ( 'NONE',  ( 26.28921445626723852, 149.7786157371718616, -3.732453678475698311 ) ) ;
#10667 = CARTESIAN_POINT ( 'NONE',  ( 42.37836782381873491, 91.71465960395167372, 14.44224817795539373 ) ) ;
#10668 = FACE_OUTER_BOUND ( 'NONE', #1496, .T. ) ;
#10669 = CARTESIAN_POINT ( 'NONE',  ( 38.58424406990785371, 78.22977050742731819, 32.77220824515697473 ) ) ;
#10670 = ORIENTED_EDGE ( 'NONE', *, *, #16732, .F. ) ;
#10671 = CARTESIAN_POINT ( 'NONE',  ( 48.01140435219951996, 61.28445800887258343, 34.21067981925357060 ) ) ;
#10672 = CARTESIAN_POINT ( 'NONE',  ( -141.4692556286852891, -172.1391397928654783, 52.90620854394536821 ) ) ;
#10673 = CARTESIAN_POINT ( 'NONE',  ( 43.01140435219951286, 133.4604996726487514, 39.46799094044489209 ) ) ;
#10675 = CARTESIAN_POINT ( 'NONE',  ( 8.886384673113061794, 121.3059481585812733, 3.129088064915290346 ) ) ;
#10674 = CARTESIAN_POINT ( 'NONE',  ( 45.74753988029933538, 80.06518717409397823, 30.44471234641811819 ) ) ;
#10676 = CARTESIAN_POINT ( 'NONE',  ( -160.8964159109769696, -182.0438272943107449, 46.59394152635518083 ) ) ;
#10677 = CARTESIAN_POINT ( 'NONE',  ( 59.73150498404358899, 90.03452709159309109, 13.76780503130795097 ) ) ;
#10678 = CARTESIAN_POINT ( 'NONE',  ( -159.5594255724347761, -190.2630981290893146, 55.53486410454104316 ) ) ;
#10679 = FACE_BOUND ( 'NONE', #13098, .T. ) ;
#10680 = DIRECTION ( 'NONE',  ( -1.000000000000000000, 0.000000000000000000, 0.000000000000000000 ) ) ;
#10681 = CARTESIAN_POINT ( 'NONE',  ( 41.64333658814960870, 144.9797705074273324, 38.42115945441014446 ) ) ;
#10682 = CARTESIAN_POINT ( 'NONE',  ( 38.58424406990784661, 105.5297705074273011, 35.64915139335016647 ) ) ;
#10683 = CARTESIAN_POINT ( 'NONE',  ( 21.90415124324598750, 92.95514585177724598, 15.07745334355238676 ) ) ;
#10684 = CARTESIAN_POINT ( 'NONE',  ( 41.64333658814960870, 135.7151871740940123, 38.42115945441014446 ) ) ;
#10685 = FACE_OUTER_BOUND ( 'NONE', #5879, .T. ) ;
#10686 = CARTESIAN_POINT ( 'NONE',  ( -157.2955611005345986, -164.6084106276440480, 41.63779006702063867 ) ) ;
#10687 = DIRECTION ( 'NONE',  ( 0.000000000000000000, 0.000000000000000000, 1.000000000000000000 ) ) ;
#10688 = CARTESIAN_POINT ( 'NONE',  ( 38.01140435219952707, 135.8604996726487002, 35.83527830041809636 ) ) ;
#10689 =( BOUNDED_CURVE ( )  B_SPLINE_CURVE ( 2, ( #500, #18908, #8781, #15496, #3814, #10540, #17241, #2155, #8890, #7236, #13937, #5559, #19021 ),
 .UNSPECIFIED., .F., .F. ) 
 B_SPLINE_CURVE_WITH_KNOTS ( ( 3, 2, 2, 2, 2, 2, 3 ),
 ( 0.3392857142857142461, 0.3428571428571428603, 0.3499999999999999778, 0.3571428571428571508, 0.3642857142857142683, 0.3714285714285714413, 0.3750000000000000000 ),
 .UNSPECIFIED. ) 
 CURVE ( )  GEOMETRIC_REPRESENTATION_ITEM ( )  RATIONAL_B_SPLINE_CURVE ( ( 0.9755282581475768211, 0.9755282581475765991, 1.000000000000000000, 0.9510565162951535312, 1.000000000000000000, 0.9510565162951535312, 1.000000000000000000, 0.9510565162951535312, 1.000000000000000000, 0.9510565162951535312, 1.000000000000000000, 0.9755282581475768211, 0.9755282581475768211 ) ) 
 REPRESENTATION_ITEM ( '' )  );
#10690 = CARTESIAN_POINT ( 'NONE',  ( 19.91114674846567922, 103.5922903064164302, 14.48528786281536895 ) ) ;
#10691 = DIRECTION ( 'NONE',  ( 0.000000000000000000, 0.000000000000000000, 1.000000000000000000 ) ) ;
#10692 = CARTESIAN_POINT ( 'NONE',  ( 41.64333658814960870, 119.5151871740940095, 30.00020018409699318 ) ) ;
#10693 = ORIENTED_EDGE ( 'NONE', *, *, #4382, .F. ) ;
#10694 = EDGE_CURVE ( 'NONE', #19966, #2116, #17834, .T. ) ;
#10695 = DIRECTION ( 'NONE',  ( 0.9385982292947089300, 0.3450121214752274734, 0.000000000000000000 ) ) ;
#10696 = ORIENTED_EDGE ( 'NONE', *, *, #5177, .F. ) ;
#10697 = CARTESIAN_POINT ( 'NONE',  ( 44.55648932407425633, 91.88445800887258486, 29.45539723777780239 ) ) ;
#10698 = CARTESIAN_POINT ( 'NONE',  ( 40.27526882409969744, 150.8297705074273267, 37.97664729208901235 ) ) ;
#10699 = ADVANCED_FACE ( 'NONE', ( #1043 ), #14699, .F. ) ;
#10700 = CARTESIAN_POINT ( 'NONE',  ( 48.01140435219951996, 155.3604996726487570, 32.58608133808903773 ) ) ;
#10702 = CARTESIAN_POINT ( 'NONE',  ( 19.10471955674299238, 134.7123306330852870, -3.220215631267630219 ) ) ;
#10701 = CARTESIAN_POINT ( 'NONE',  ( 44.37947211624943833, 119.2151871740939981, 30.00020018409699318 ) ) ;
#10703 = EDGE_CURVE ( 'NONE', #17373, #13772, #6101, .T. ) ;
#10704 = CARTESIAN_POINT ( 'NONE',  ( 44.55648932407425633, 68.81049967264874567, 29.45539723777780239 ) ) ;
#10706 = CYLINDRICAL_SURFACE ( 'NONE', #14629, 4.999999999999997335 ) ;
#10705 = CARTESIAN_POINT ( 'NONE',  ( 43.01140435219951286, 77.96049967264873715, 29.21067981925356705 ) ) ;
#10707 = CARTESIAN_POINT ( 'NONE',  ( 147.8787791192428074, -126.9891397928655010, 49.65701158161629536 ) ) ;
#10708 = CARTESIAN_POINT ( 'NONE',  ( 38.01140435219952707, 123.8604996726487570, 35.83527830041809636 ) ) ;
#10709 = CARTESIAN_POINT ( 'NONE',  ( 45.22896085152458312, 95.00377825571473522, 29.71740844387221969 ) ) ;
#10710 = CARTESIAN_POINT ( 'NONE',  ( 43.01140435219951286, 69.86518717409400381, 38.86567161673127657 ) ) ;
#10711 = CARTESIAN_POINT ( 'NONE',  ( 147.5268905834513475, 193.0332408774651185, -44.99999999999997158 ) ) ;
#10712 = CARTESIAN_POINT ( 'NONE',  ( -148.5561028927606344, -182.7938272943107449, 40.69124936498395328 ) ) ;
#10713 = CARTESIAN_POINT ( 'NONE',  ( -142.0420953463936087, -192.6584106276440593, 49.65701158161630957 ) ) ;
#10714 = EDGE_LOOP ( 'NONE', ( #4667, #6825, #11939, #16128 ) ) ;
#10715 = CARTESIAN_POINT ( 'NONE',  ( -151.4692556286852891, -175.4084106276440878, 59.56931450028537967 ) ) ;
#10716 = CARTESIAN_POINT ( 'NONE',  ( 9.433072040199128594, 112.8364229897773470, 7.858512901693939234 ) ) ;
#10717 = ORIENTED_EDGE ( 'NONE', *, *, #1256, .T. ) ;
#10718 = CARTESIAN_POINT ( 'NONE',  ( 39.42975644700377558, 141.4151871740940010, 36.81289934271958941 ) ) ;
#10719 = CARTESIAN_POINT ( 'NONE',  ( 41.64333658814960870, 101.7797705074273154, 30.00020018409699318 ) ) ;
#10720 = VERTEX_POINT ( 'NONE', #2801 ) ;
#10721 = ORIENTED_EDGE ( 'NONE', *, *, #21484, .T. ) ;
#10722 = ADVANCED_FACE ( 'NONE', ( #9540 ), #1257, .F. ) ;
#10723 = CARTESIAN_POINT ( 'NONE',  ( 24.25535704844963547, 98.85002770340597067, 1.227849354118501601 ) ) ;
#10724 = ORIENTED_EDGE ( 'NONE', *, *, #1261, .F. ) ;
#10725 = CARTESIAN_POINT ( 'NONE',  ( 48.01140435219951996, 115.2844580088725763, 34.21067981925357060 ) ) ;
#10726 = AXIS2_PLACEMENT_3D ( 'NONE', #2428, #14323, #12675 ) ;
#10727 = LINE ( 'NONE', #5750, #1997 ) ;
#10728 = EDGE_CURVE ( 'NONE', #5083, #21052, #19666, .T. ) ;
#10729 = CARTESIAN_POINT ( 'NONE',  ( 46.59305225739526435, 82.57977050742731251, 36.81289934271958941 ) ) ;
#10730 = CARTESIAN_POINT ( 'NONE',  ( 38.58424406990786082, 144.1151871740939896, 34.21067981925357060 ) ) ;
#10731 = CARTESIAN_POINT ( 'NONE',  ( 48.01140435219951996, 101.0604996726487173, 35.83527830041810347 ) ) ;
#10732 = CARTESIAN_POINT ( 'NONE',  ( 12.03843011909301453, 134.4860913190374561, 2.577281550626734141 ) ) ;
#10733 = FACE_OUTER_BOUND ( 'NONE', #18497, .T. ) ;
#10734 = CARTESIAN_POINT ( 'NONE',  ( -141.4692556286852891, -174.9891397928654726, 49.65701158161630957 ) ) ;
#10735 = CARTESIAN_POINT ( 'NONE',  ( 44.55648932407425633, 64.88445800887257064, 29.45539723777780239 ) ) ;
#10736 = CARTESIAN_POINT ( 'NONE',  ( -159.5594255724347761, -163.8630981290893089, 43.77915905869157598 ) ) ;
#10737 = ORIENTED_EDGE ( 'NONE', *, *, #2276, .T. ) ;
#10738 = CARTESIAN_POINT ( 'NONE',  ( 47.43856463449118621, 85.87977050742730967, 34.21067981925357060 ) ) ;
#10739 = CARTESIAN_POINT ( 'NONE',  ( -160.8964159109769696, -160.7438272943107052, 52.72008163687743121 ) ) ;
#10740 = CARTESIAN_POINT ( 'NONE',  ( 38.58424406990785371, 68.96518717409398391, 32.77220824515697473 ) ) ;
#10741 = FACE_OUTER_BOUND ( 'NONE', #11032, .T. ) ;
#10742 = CYLINDRICAL_SURFACE ( 'NONE', #4441, 4.999999999999997335 ) ;
#10743 = ORIENTED_EDGE ( 'NONE', *, *, #3467, .T. ) ;
#10744 = CARTESIAN_POINT ( 'NONE',  ( 134.6380592378699532, 268.5785371414991687, -19.99999999999997868 ) ) ;
#10745 = DIRECTION ( 'NONE',  ( 0.000000000000000000, -1.000000000000000000, 0.000000000000000000 ) ) ;
#10746 = CARTESIAN_POINT ( 'NONE',  ( 47.43856463449118621, 136.8797705074273381, 34.21067981925357060 ) ) ;
#10747 = CARTESIAN_POINT ( 'NONE',  ( 33.35040633798650589, 93.49848361726675705, 8.803757759246650494 ) ) ;
#10748 = ORIENTED_EDGE ( 'NONE', *, *, #17540, .T. ) ;
#10749 = DIRECTION ( 'NONE',  ( -0.000000000000000000, 1.000000000000000000, -0.000000000000000000 ) ) ;
#10750 = EDGE_LOOP ( 'NONE', ( #21683, #21075, #4887, #17366 ) ) ;
#10751 = CARTESIAN_POINT ( 'NONE',  ( 47.43856463449117200, 136.7297705074272756, 35.64915139335016647 ) ) ;
#10752 = CARTESIAN_POINT ( 'NONE',  ( 47.05648932407426344, 154.9104996726487400, 37.14960608071593384 ) ) ;
#10753 = CARTESIAN_POINT ( 'NONE',  ( 42.21948215057684450, 110.1113394311928175, 29.21067981925355994 ) ) ;
#10754 = CARTESIAN_POINT ( 'NONE',  ( -158.9748091281504401, -116.9891397928655010, 62.65701158161630957 ) ) ;
#10755 = CARTESIAN_POINT ( 'NONE',  ( 163.1026836591718734, 192.4288937294299160, 24.47866928663567521 ) ) ;
#10756 = CARTESIAN_POINT ( 'NONE',  ( 40.27526882409969033, 98.66518717409400097, 30.44471234641811819 ) ) ;
#10757 = CARTESIAN_POINT ( 'NONE',  ( 46.10157429594899270, 132.8344580088725593, 38.46393386101375711 ) ) ;
#10758 = DIRECTION ( 'NONE',  ( 0.000000000000000000, 0.000000000000000000, 1.000000000000000000 ) ) ;
#10759 = CARTESIAN_POINT ( 'NONE',  ( -141.4692556286852891, -155.9130981290893203, 46.40781461928724383 ) ) ;
#10760 = DIRECTION ( 'NONE',  ( 0.1884548733085491812, -2.775557561562891351E-17, 0.9820818503191364179 ) ) ;
#10761 = VECTOR ( 'NONE', #9692, 1000.000000000000000 ) ;
#10762 = CARTESIAN_POINT ( 'NONE',  ( 44.55648932407425633, 71.81049967264874567, 29.45539723777780239 ) ) ;
#10763 = CARTESIAN_POINT ( 'NONE',  ( 38.01140435219951996, 128.6344580088725706, 32.58608133808903773 ) ) ;
#10764 = CARTESIAN_POINT ( 'NONE',  ( 45.74753988029933538, 116.3297705074272983, 30.44471234641811819 ) ) ;
#10765 = CARTESIAN_POINT ( 'NONE',  ( 70.23874406963963679, 127.5525917602273012, 4.366313592093098883 ) ) ;
#10766 = CARTESIAN_POINT ( 'NONE',  ( -160.8964159109769696, -193.7438272943106767, 52.72008163687743121 ) ) ;
#10767 = CARTESIAN_POINT ( 'NONE',  ( 47.43856463449118621, 103.6151871740940038, 34.21067981925357060 ) ) ;
#10768 = LINE ( 'NONE', #2591, #7541 ) ;
#10769 = ORIENTED_EDGE ( 'NONE', *, *, #17566, .T. ) ;
#10770 = CARTESIAN_POINT ( 'NONE',  ( -56.84366818088135176, 789.5005544000622422, -19.99999999999997868 ) ) ;
#10771 = CARTESIAN_POINT ( 'NONE',  ( 49.23863765798637360, 86.32632880410874066, 8.129368652084252744 ) ) ;
#10772 = CARTESIAN_POINT ( 'NONE',  ( 71.19791805076843616, 120.7596060772701776, 5.632536115698772328 ) ) ;
#10773 = EDGE_CURVE ( 'NONE', #4323, #18099, #19251, .T. ) ;
#10774 = CARTESIAN_POINT ( 'NONE',  ( 43.01140435219954838, 108.5344580088725763, 39.21067981925356349 ) ) ;
#10775 = CARTESIAN_POINT ( 'NONE',  ( 47.43856463449118621, 79.87977050742732388, 34.21067981925357060 ) ) ;
#10776 = VERTEX_POINT ( 'NONE', #13053 ) ;
#10777 = VERTEX_POINT ( 'NONE', #19779 ) ;
#10778 = VECTOR ( 'NONE', #11621, 1000.000000000000000 ) ;
#10779 = CARTESIAN_POINT ( 'NONE',  ( -151.4692556286852607, -165.8130981290893260, 59.65701158161632378 ) ) ;
#10780 = CARTESIAN_POINT ( 'NONE',  ( 43.01140435219951286, 124.4604996726487371, 39.46799094044489209 ) ) ;
#10782 = CARTESIAN_POINT ( 'NONE',  ( 18.41688673663920284, 143.6040338654656523, -3.061295755333778512 ) ) ;
#10781 = CARTESIAN_POINT ( 'NONE',  ( 41.64333658814960870, 81.71518717409399812, 38.42115945441014446 ) ) ;
#10783 = CARTESIAN_POINT ( 'NONE',  ( -157.2955611005345986, -173.3438272943107279, 41.63779006702063867 ) ) ;
#10784 = CARTESIAN_POINT ( 'NONE',  ( 9.203281625063985061, 114.5318647093721864, 15.91056058043385413 ) ) ;
#10785 = CARTESIAN_POINT ( 'NONE',  ( -151.4692556286852891, -191.3130981290893260, 39.14238933923362396 ) ) ;
#10786 = CARTESIAN_POINT ( 'NONE',  ( 38.01140435219952707, 80.63445800887257064, 32.58608133808903773 ) ) ;
#10787 = CYLINDRICAL_SURFACE ( 'NONE', #21652, 7.500000000000007105 ) ;
#10788 = CARTESIAN_POINT ( 'NONE',  ( 41.46631938032478359, 158.1844580088726104, 29.45539723777780239 ) ) ;
#10789 = CARTESIAN_POINT ( 'NONE',  ( 39.42975644700377558, 141.6797705074273210, 36.81289934271958941 ) ) ;
#10790 = CARTESIAN_POINT ( 'NONE',  ( 40.23585178891228509, 85.70481357498144348, 6.429941473113898631 ) ) ;
#10791 = CARTESIAN_POINT ( 'NONE',  ( 40.27526882409969744, 131.6651871740939725, 30.44471234641812174 ) ) ;
#10792 = AXIS2_PLACEMENT_3D ( 'NONE', #11561, #104, #5590 ) ;
#10793 = CARTESIAN_POINT ( 'NONE',  ( 41.46631938032478359, 70.31049967264874567, 38.96596240072933170 ) ) ;
#10794 = CARTESIAN_POINT ( 'NONE',  ( -157.2955611005345986, -167.6084106276440195, 41.63779006702063867 ) ) ;
#10795 = CARTESIAN_POINT ( 'NONE',  ( -27.64582385433943656, -34.13255853780189142, 5.000000000000018652 ) ) ;
#10796 = VECTOR ( 'NONE', #20350, 1000.000000000000000 ) ;
#10797 = CARTESIAN_POINT ( 'NONE',  ( 46.10157429594899270, 91.73445800887257917, 29.95742577749336988 ) ) ;
#10798 = CARTESIAN_POINT ( 'NONE',  ( 15.34898554898258460, 114.0222161449793248, 7.937823431466153323 ) ) ;
#10799 = CARTESIAN_POINT ( 'NONE',  ( 43.01140435219951996, 10.71049967264875491, 34.21067981925357060 ) ) ;
#10800 = CARTESIAN_POINT ( 'NONE',  ( 45.74753988029933538, 113.0651871740939924, 30.44471234641811819 ) ) ;
#10801 = VERTEX_POINT ( 'NONE', #4672 ) ;
#10802 = CARTESIAN_POINT ( 'NONE',  ( -157.6495955161842062, -160.1130981290893089, 58.16351966513671812 ) ) ;
#10803 = EDGE_CURVE ( 'NONE', #21295, #5138, #19605, .T. ) ;
#10804 = VERTEX_POINT ( 'NONE', #16680 ) ;
#10805 = CARTESIAN_POINT ( 'NONE',  ( 43.01140435219951286, 89.03445800887256212, 28.95336869806222779 ) ) ;
#10806 = VECTOR ( 'NONE', #5837, 1000.000000000000000 ) ;
#10807 = CARTESIAN_POINT ( 'NONE',  ( 43.01140435219951286, 148.1297705074272812, 38.86567161673127657 ) ) ;
#10808 = CARTESIAN_POINT ( 'NONE',  ( 44.55648932407425633, 148.6104996726487570, 38.96596240072933170 ) ) ;
#10810 = CARTESIAN_POINT ( 'NONE',  ( 18.82712405543679779, 105.5606057458561793, -11.43438524559667790 ) ) ;
#10809 = CARTESIAN_POINT ( 'NONE',  ( 44.37947211624943833, 109.0151871740940095, 38.42115945441014446 ) ) ;
#10811 = CARTESIAN_POINT ( 'NONE',  ( 38.01140435219951996, 75.56049967264871725, 32.58608133808903773 ) ) ;
#10813 = CARTESIAN_POINT ( 'NONE',  ( 46.10157429594899270, 61.73445800887256496, 29.95742577749336988 ) ) ;
#10812 = DIRECTION ( 'NONE',  ( 0.8302490056034133037, 0.5573926701119628069, -9.854660648260994945E-17 ) ) ;
#10814 = CARTESIAN_POINT ( 'NONE',  ( 43.01140435219951286, 85.46049967264872294, 39.21067981925356349 ) ) ;
#10815 = CARTESIAN_POINT ( 'NONE',  ( 32.23767430054768823, 145.5917660130458842, 17.43780275515694456 ) ) ;
#10816 = CARTESIAN_POINT ( 'NONE',  ( -56.84366818088135176, 789.5005544000622422, -19.99999999999997868 ) ) ;
#10817 =( BOUNDED_CURVE ( )  B_SPLINE_CURVE ( 2, ( #5952, #8849, #12680, #783, #5515, #9172, #3879, #5739, #4090, #3771, #7518, #10604, #17308, #2112, #19088, #2220, #17632, #15770, #15556, #7190, #10713, #13895, #14219, #15870, #8950, #17416, #15978, #14005, #2540, #20633, #20959, #7304, #9277, #20739, #3988, #12462, #2321, #9060, #7410, #674, #10821, #9499, #1215, #8057, #12900, #4515, #19843, #4734, #19733, #2758, #11453, #4626, #21506, #7949, #13012, #16520, #7737, #6280, #19402, #16414, #11345, #18182, #16196, #21172, #2975, #14438, #11133, #11025, #1108, #2643, #9713, #6063, #8166, #18068, #1436, #9822, #1324, #19509, #16305, #14872, #17737, #21287, #14763, #4402, #19621, #11238, #3089, #21617, #6393, #7843, #6508, #13121, #4298, #14654, #9385, #16090, #12790, #1000, #17848, #14545, #6166, #17958, #2863, #9606, #21394, #1547, #4966, #4850, #18412, #18299, #18628, #14979, #1981, #13550, #10366, #3640, #10258, #13342, #10150, #8714, #11570, #15097, #16960, #20079, #5075, #329, #16746, #1, #3533, #10042, #6742, #1872, #20392, #13450, #17067, #5289, #216, #1656, #112, #6952, #1766, #20287, #8388, #15213, #3429, #6844, #3201, #11678, #5181, #8602, #15322, #15433, #11900, #13228, #16636, #21724, #3312, #6628, #20184, #11789, #13659, #9931, #8278, #12003, #18520, #19965, #16851, #8500, #18737, #8823, #20823, #438, #9036, #651, #7059, #4065, #7168, #13871, #4175, #15632, #20609, #19165, #10903, #10477, #2409, #17607, #18841, #10794, #5714, #5492, #20716, #19274, #17282, #14194, #17177, #12439, #5393, #20934, #2090, #12219, #17392, #5600, #12326, #5815, #2513, #15846, #18953, #10686, #17498, #9146, #15532, #757, #3854, #15746, #7387, #13763, #7493, #10579, #2197, #9253, #537, #12546, #15953, #20505, #8927, #12109, #3747, #7277, #13978, #19061, #3964, #2295, #14087, #11106, #8032, #4273, #6253, #21044, #14739, #17712, #971, #9355, #4598, #4484, #19591, #11212, #21149, #5927, #9798, #7921, #12656, #17820, #19707, #21363, #19378, #16282, #9688, #18151, #11002, #12763, #11317, #2617, #9577, #864, #18041, #1188, #12872, #7600, #19484 ),
 .UNSPECIFIED., .F., .F. ) 
 B_SPLINE_CURVE_WITH_KNOTS ( ( 3, 2, 2, 2, 2, 2, 2, 2, 2, 2, 2, 2, 2, 2, 2, 2, 2, 2, 2, 2, 2, 2, 2, 2, 2, 2, 2, 2, 2, 2, 2, 2, 2, 2, 2, 2, 2, 2, 2, 2, 2, 2, 2, 2, 2, 2, 2, 2, 2, 2, 2, 2, 2, 2, 2, 2, 2, 2, 2, 2, 2, 2, 2, 2, 2, 2, 2, 2, 2, 2, 2, 2, 2, 2, 2, 2, 2, 2, 2, 2, 2, 2, 2, 2, 2, 2, 2, 2, 2, 2, 2, 2, 2, 2, 2, 2, 2, 2, 2, 2, 2, 2, 2, 2, 2, 2, 2, 2, 2, 2, 2, 2, 2, 2, 2, 2, 2, 2, 2, 2, 2, 2, 2, 2, 2, 2, 2, 2, 2, 2, 2, 2, 2, 2, 3 ),
 ( 0.000000000000000000, 0.007142857142857142634, 0.01428571428571428527, 0.02142857142857142877, 0.02857142857142857054, 0.03571428571428571230, 0.04285714285714285754, 0.05000000000000000278, 0.05714285714285714107, 0.06428571428571427937, 0.07142857142857142461, 0.07857142857142856984, 0.08571428571428571508, 0.09285714285714286031, 0.1000000000000000056, 0.1071428571428571369, 0.1142857142857142821, 0.1214285714285714274, 0.1285714285714285587, 0.1357142857142857040, 0.1428571428571428492, 0.1499999999999999944, 0.1571428571428571397, 0.1642857142857142849, 0.1714285714285714302, 0.1785714285714285754, 0.1857142857142857206, 0.1928571428571428659, 0.2000000000000000111, 0.2071428571428571563, 0.2142857142857142738, 0.2214285714285714191, 0.2285714285714285643, 0.2357142857142857095, 0.2428571428571428548, 0.2500000000000000000, 0.2571428571428571175, 0.2642857142857142905, 0.2714285714285714080, 0.2785714285714285809, 0.2857142857142856984, 0.2928571428571428714, 0.2999999999999999889, 0.3071428571428571619, 0.3142857142857142794, 0.3214285714285713969, 0.3285714285714285698, 0.3357142857142856873, 0.3428571428571428603, 0.3499999999999999778, 0.3571428571428571508, 0.3642857142857142683, 0.3714285714285714413, 0.3785714285714285587, 0.3857142857142857317, 0.3928571428571429047, 0.4000000000000000222, 0.4071428571428571397, 0.4142857142857143127, 0.4214285714285714302, 0.4285714285714285476, 0.4357142857142857206, 0.4428571428571428381, 0.4500000000000000111, 0.4571428571428571286, 0.4642857142857142461, 0.4714285714285714191, 0.4785714285714285920, 0.4857142857142857095, 0.4928571428571428825, 0.5000000000000000000, 0.5071428571428571175, 0.5142857142857142350, 0.5214285714285714635, 0.5285714285714285809, 0.5357142857142856984, 0.5428571428571428159, 0.5500000000000000444, 0.5571428571428571619, 0.5642857142857142794, 0.5714285714285713969, 0.5785714285714286254, 0.5857142857142857428, 0.5928571428571428603, 0.5999999999999999778, 0.6071428571428570953, 0.6142857142857143238, 0.6214285714285714413, 0.6285714285714285587, 0.6357142857142856762, 0.6428571428571427937, 0.6500000000000000222, 0.6571428571428571397, 0.6642857142857142572, 0.6714285714285713746, 0.6785714285714286031, 0.6857142857142857206, 0.6928571428571428381, 0.6999999999999999556, 0.7071428571428571841, 0.7142857142857143016, 0.7214285714285714191, 0.7285714285714285365, 0.7357142857142857650, 0.7428571428571428825, 0.7500000000000000000, 0.7571428571428571175, 0.7642857142857142350, 0.7714285714285714635, 0.7785714285714285809, 0.7857142857142858094, 0.7928571428571428159, 0.8000000000000000444, 0.8071428571428571619, 0.8142857142857142794, 0.8214285714285713969, 0.8285714285714286254, 0.8357142857142857428, 0.8428571428571428603, 0.8499999999999999778, 0.8571428571428570953, 0.8642857142857143238, 0.8714285714285714413, 0.8785714285714285587, 0.8857142857142856762, 0.8928571428571429047, 0.9000000000000000222, 0.9071428571428571397, 0.9142857142857142572, 0.9214285714285713746, 0.9285714285714284921, 0.9357142857142857206, 0.9428571428571428381, 0.9499999999999999556, 0.9523897249335834259 ),
 .UNSPECIFIED. ) 
 CURVE ( )  GEOMETRIC_REPRESENTATION_ITEM ( )  RATIONAL_B_SPLINE_CURVE ( ( 1.000000000000000000, 0.9510565162951535312, 1.000000000000000000, 0.9510565162951535312, 1.000000000000000000, 0.9510565162951535312, 1.000000000000000000, 0.9510565162951535312, 1.000000000000000000, 0.9510565162951535312, 1.000000000000000000, 0.9510565162951535312, 1.000000000000000000, 0.9510565162951535312, 1.000000000000000000, 0.9510565162951535312, 1.000000000000000000, 0.9510565162951535312, 1.000000000000000000, 0.9510565162951535312, 1.000000000000000000, 0.9510565162951535312, 1.000000000000000000, 0.9510565162951535312, 1.000000000000000000, 0.9510565162951535312, 1.000000000000000000, 0.9510565162951535312, 1.000000000000000000, 0.9510565162951535312, 1.000000000000000000, 0.9510565162951535312, 1.000000000000000000, 0.9510565162951535312, 1.000000000000000000, 0.9510565162951535312, 1.000000000000000000, 0.9510565162951535312, 1.000000000000000000, 0.9510565162951535312, 1.000000000000000000, 0.9510565162951535312, 1.000000000000000000, 0.9510565162951535312, 1.000000000000000000, 0.9510565162951535312, 1.000000000000000000, 0.9510565162951535312, 1.000000000000000000, 0.9510565162951535312, 1.000000000000000000, 0.9510565162951535312, 1.000000000000000000, 0.9510565162951535312, 1.000000000000000000, 0.9510565162951535312, 1.000000000000000000, 0.9510565162951535312, 1.000000000000000000, 0.9510565162951535312, 1.000000000000000000, 0.9510565162951535312, 1.000000000000000000, 0.9510565162951535312, 1.000000000000000000, 0.9510565162951535312, 1.000000000000000000, 0.9510565162951535312, 1.000000000000000000, 0.9510565162951535312, 1.000000000000000000, 0.9510565162951535312, 1.000000000000000000, 0.9510565162951535312, 1.000000000000000000, 0.9510565162951535312, 1.000000000000000000, 0.9510565162951535312, 1.000000000000000000, 0.9510565162951535312, 1.000000000000000000, 0.9510565162951535312, 1.000000000000000000, 0.9510565162951535312, 1.000000000000000000, 0.9510565162951535312, 1.000000000000000000, 0.9510565162951535312, 1.000000000000000000, 0.9510565162951535312, 1.000000000000000000, 0.9510565162951535312, 1.000000000000000000, 0.9510565162951535312, 1.000000000000000000, 0.9510565162951535312, 1.000000000000000000, 0.9510565162951535312, 1.000000000000000000, 0.9510565162951535312, 1.000000000000000000, 0.9510565162951535312, 1.000000000000000000, 0.9510565162951535312, 1.000000000000000000, 0.9510565162951535312, 1.000000000000000000, 0.9510565162951535312, 1.000000000000000000, 0.9510565162951535312, 1.000000000000000000, 0.9510565162951535312, 1.000000000000000000, 0.9510565162951535312, 1.000000000000000000, 0.9510565162951535312, 1.000000000000000000, 0.9510565162951535312, 1.000000000000000000, 0.9510565162951535312, 1.000000000000000000, 0.9510565162951535312, 1.000000000000000000, 0.9510565162951535312, 1.000000000000000000, 0.9510565162951535312, 1.000000000000000000, 0.9510565162951535312, 1.000000000000000000, 0.9510565162951535312, 1.000000000000000000, 0.9510565162951535312, 1.000000000000000000, 0.9510565162951535312, 1.000000000000000000, 0.9510565162951535312, 1.000000000000000000, 0.9510565162951535312, 1.000000000000000000, 0.9510565162951535312, 1.000000000000000000, 0.9510565162951535312, 1.000000000000000000, 0.9510565162951535312, 1.000000000000000000, 0.9510565162951535312, 1.000000000000000000, 0.9510565162951535312, 1.000000000000000000, 0.9510565162951535312, 1.000000000000000000, 0.9510565162951535312, 1.000000000000000000, 0.9510565162951535312, 1.000000000000000000, 0.9510565162951535312, 1.000000000000000000, 0.9510565162951535312, 1.000000000000000000, 0.9510565162951535312, 1.000000000000000000, 0.9510565162951535312, 1.000000000000000000, 0.9510565162951535312, 1.000000000000000000, 0.9510565162951535312, 1.000000000000000000, 0.9510565162951535312, 1.000000000000000000, 0.9510565162951535312, 1.000000000000000000, 0.9510565162951535312, 1.000000000000000000, 0.9510565162951535312, 1.000000000000000000, 0.9510565162951535312, 1.000000000000000000, 0.9510565162951535312, 1.000000000000000000, 0.9510565162951535312, 1.000000000000000000, 0.9510565162951535312, 1.000000000000000000, 0.9510565162951535312, 1.000000000000000000, 0.9510565162951535312, 1.000000000000000000, 0.9510565162951535312, 1.000000000000000000, 0.9510565162951535312, 1.000000000000000000, 0.9510565162951535312, 1.000000000000000000, 0.9510565162951535312, 1.000000000000000000, 0.9510565162951535312, 1.000000000000000000, 0.9510565162951535312, 1.000000000000000000, 0.9510565162951535312, 1.000000000000000000, 0.9510565162951535312, 1.000000000000000000, 0.9510565162951535312, 1.000000000000000000, 0.9510565162951535312, 1.000000000000000000, 0.9510565162951535312, 1.000000000000000000, 0.9510565162951535312, 1.000000000000000000, 0.9510565162951535312, 1.000000000000000000, 0.9510565162951535312, 1.000000000000000000, 0.9510565162951535312, 1.000000000000000000, 0.9510565162951535312, 1.000000000000000000, 0.9510565162951535312, 1.000000000000000000, 0.9510565162951535312, 1.000000000000000000, 0.9510565162951535312, 1.000000000000000000, 0.9510565162951535312, 1.000000000000000000, 0.9510565162951535312, 1.000000000000000000, 0.9510565162951535312, 1.000000000000000000, 0.9510565162951535312, 1.000000000000000000, 0.9510565162951535312, 1.000000000000000000, 0.9510565162951535312, 1.000000000000000000, 0.9510565162951535312, 1.000000000000000000, 0.9510565162951535312, 1.000000000000000000, 0.9510565162951535312, 1.000000000000000000, 0.9510565162951535312, 1.000000000000000000, 0.9510565162951535312, 1.000000000000000000, 0.9510565162951535312, 1.000000000000000000, 0.9510565162951535312, 1.000000000000000000, 0.9510565162951535312, 1.000000000000000000, 0.9510565162951535312, 1.000000000000000000, 0.9510565162951535312, 1.000000000000000000, 0.9510565162951535312, 1.000000000000000000, 0.9510565162951535312, 1.000000000000000000, 0.9510565162951535312, 1.000000000000000000, 0.9510565162951535312, 1.000000000000000000, 0.9510565162951535312, 1.000000000000000000, 0.9836253951315730992, 0.9782074146920101132 ) ) 
 REPRESENTATION_ITEM ( '' )  );
#10818 = CARTESIAN_POINT ( 'NONE',  ( 45.74753988029933538, 67.16518717409401518, 37.97664729208901946 ) ) ;
#10819 = CARTESIAN_POINT ( 'NONE',  ( 47.05648932407426344, 104.5104996726487485, 31.27175355779120025 ) ) ;
#10820 = CARTESIAN_POINT ( 'NONE',  ( -143.8425227516148084, -183.6938272943107506, 55.19815736654470584 ) ) ;
#10821 = CARTESIAN_POINT ( 'NONE',  ( -142.0420953463936087, -189.6584106276440593, 49.65701158161630957 ) ) ;
#10822 = EDGE_CURVE ( 'NONE', #19334, #602, #947, .T. ) ;
#10823 = EDGE_LOOP ( 'NONE', ( #18559, #19410, #10961, #21055 ) ) ;
#10824 = CARTESIAN_POINT ( 'NONE',  ( -142.0420953463936087, -174.6584106276440593, 49.65701158161630957 ) ) ;
#10825 = VECTOR ( 'NONE', #10812, 1000.000000000000114 ) ;
#10826 = CARTESIAN_POINT ( 'NONE',  ( 17.52475135776945336, 142.8823211630961794, 1.906181796079885027 ) ) ;
#10827 = VERTEX_POINT ( 'NONE', #13888 ) ;
#10828 = CARTESIAN_POINT ( 'NONE',  ( 47.43856463449117200, 142.4651871740940123, 35.64915139335016647 ) ) ;
#10829 = CARTESIAN_POINT ( 'NONE',  ( 39.42975644700377558, 155.8151871740940067, 31.60846029578754468 ) ) ;
#10830 = ADVANCED_FACE ( 'NONE', ( #1999 ), #1590, .F. ) ;
#10831 = CARTESIAN_POINT ( 'NONE',  ( 46.59305225739526435, 107.1797705074273352, 31.60846029578754468 ) ) ;
#10832 = ORIENTED_EDGE ( 'NONE', *, *, #15168, .T. ) ;
#10833 = ORIENTED_EDGE ( 'NONE', *, *, #5579, .T. ) ;
#10834 = CARTESIAN_POINT ( 'NONE',  ( 18.92353847440636727, 134.5693106245527702, 2.775393258647981920 ) ) ;
#10835 = VERTEX_POINT ( 'NONE', #8943 ) ;
#10836 = CARTESIAN_POINT ( 'NONE',  ( 48.01140435219951996, 115.1344580088725849, 35.83527830041810347 ) ) ;
#10837 = AXIS2_PLACEMENT_3D ( 'NONE', #12350, #3986, #5841 ) ;
#10838 = CARTESIAN_POINT ( 'NONE',  ( 43.01140435219951286, 76.46049967264873715, 39.21067981925356349 ) ) ;
#10839 = CARTESIAN_POINT ( 'NONE',  ( 41.64333658814960870, 81.97977050742731819, 38.42115945441014446 ) ) ;
#10840 = CARTESIAN_POINT ( 'NONE',  ( 39.42975644700377558, 138.4151871740940010, 36.81289934271958941 ) ) ;
#10841 = AXIS2_PLACEMENT_3D ( 'NONE', #14352, #9408, #15998 ) ;
#10842 = CARTESIAN_POINT ( 'NONE',  ( 38.01140435219951996, 99.56049967264873146, 32.58608133808903773 ) ) ;
#10843 = CARTESIAN_POINT ( 'NONE',  ( 14.88286428391304561, 100.3963227437532595, 8.410691821786379307 ) ) ;
#10844 = CARTESIAN_POINT ( 'NONE',  ( -151.4692556286853176, -179.3130981290892976, 39.65701158161629536 ) ) ;
#10845 = CARTESIAN_POINT ( 'NONE',  ( -151.4692556286852891, -171.2391397928654442, 39.14238933923362396 ) ) ;
#10846 = CARTESIAN_POINT ( 'NONE',  ( -141.4692556286852891, -159.2130981290893033, 52.90620854394536821 ) ) ;
#10847 = CARTESIAN_POINT ( 'NONE',  ( 43.01140435219951286, 94.90707761860558378, 39.21067981925356349 ) ) ;
#10848 = APPLICATION_CONTEXT ( 'automotive_design' ) ;
#10849 = PLANE ( 'NONE',  #4998 ) ;
#10850 = ORIENTED_EDGE ( 'NONE', *, *, #868, .T. ) ;
#10851 = CARTESIAN_POINT ( 'NONE',  ( 39.42975644700377558, 81.07977050742731251, 31.60846029578754468 ) ) ;
#10852 = CARTESIAN_POINT ( 'NONE',  ( -160.8964159109769696, -161.0438272943107449, 46.59394152635518793 ) ) ;
#10853 = CARTESIAN_POINT ( 'NONE',  ( 40.27526882409969744, 65.66518717409398675, 30.44471234641812174 ) ) ;
#10854 = CARTESIAN_POINT ( 'NONE',  ( 66.76198117565915879, 95.25264312590786631, -0.5179092472497510702 ) ) ;
#10855 = CYLINDRICAL_SURFACE ( 'NONE', #10101, 10.00000000000000888 ) ;
#10856 = VERTEX_POINT ( 'NONE', #18856 ) ;
#10857 = CARTESIAN_POINT ( 'NONE',  ( 38.01140435219952707, 68.78445800887257633, 34.21067981925357060 ) ) ;
#10858 = DIRECTION ( 'NONE',  ( -0.000000000000000000, -0.000000000000000000, 1.000000000000000000 ) ) ;
#10859 = CARTESIAN_POINT ( 'NONE',  ( 38.58424406990785371, 135.5297705074273154, 35.64915139335015937 ) ) ;
#10860 = CARTESIAN_POINT ( 'NONE',  ( 65.57965399412842089, 103.1314161556117028, 7.375186511277089352 ) ) ;
#10861 = VERTEX_POINT ( 'NONE', #5509 ) ;
#10862 = CARTESIAN_POINT ( 'NONE',  ( 111.4021762516569964, 137.5714195593754710, 4.000000000000021316 ) ) ;
#10863 = VERTEX_POINT ( 'NONE', #18969 ) ;
#10864 = CARTESIAN_POINT ( 'NONE',  ( 46.59305225739526435, 128.1797705074273210, 31.60846029578754468 ) ) ;
#10865 = CARTESIAN_POINT ( 'NONE',  ( 43.01140435219954838, 110.9604996726487371, 29.21067981925356705 ) ) ;
#10866 = CARTESIAN_POINT ( 'NONE',  ( -151.4692556286852891, -196.9891397928655010, 59.65701158161632378 ) ) ;
#10867 = DIRECTION ( 'NONE',  ( -0.000000000000000000, -0.000000000000000000, 1.000000000000000000 ) ) ;
#10868 = CARTESIAN_POINT ( 'NONE',  ( 44.37947211624943833, 101.2151871740939981, 30.00020018409699318 ) ) ;
#10869 = DIRECTION ( 'NONE',  ( 7.372372188207634192E-16, 0.000000000000000000, -1.000000000000000000 ) ) ;
#10870 = CARTESIAN_POINT ( 'NONE',  ( 147.5268905834513475, 193.0332408774651185, -50.99999999999998579 ) ) ;
#10871 = CARTESIAN_POINT ( 'NONE',  ( -156.4692864601532847, -155.0638355923473739, 40.99677534440144910 ) ) ;
#10872 = SHAPE_DEFINITION_REPRESENTATION ( #4979, #1720 ) ;
#10873 = ADVANCED_FACE ( 'NONE', ( #13780 ), #3056, .T. ) ;
#10874 = CARTESIAN_POINT ( 'NONE',  ( -151.4692556286852891, -196.9891397928655010, 49.65701158161630957 ) ) ;
#10875 = CARTESIAN_POINT ( 'NONE',  ( 46.10157429594899270, 129.8344580088725877, 38.46393386101376421 ) ) ;
#10876 = CARTESIAN_POINT ( 'NONE',  ( 39.42975644700377558, 111.6797705074273210, 36.81289934271958941 ) ) ;
#10877 = CARTESIAN_POINT ( 'NONE',  ( 24.36338960932843634, 98.64599907776933208, 7.223456449276175029 ) ) ;
#10878 = CARTESIAN_POINT ( 'NONE',  ( -154.3824083646099439, -194.4938272943107336, 40.69124936498395328 ) ) ;
#10879 = CARTESIAN_POINT ( 'NONE',  ( 45.74753988029934249, 94.16518717409400097, 37.97664729208901235 ) ) ;
#10880 = DIRECTION ( 'NONE',  ( 0.000000000000000000, 0.000000000000000000, -1.000000000000000000 ) ) ;
#10881 = ORIENTED_EDGE ( 'NONE', *, *, #12868, .F. ) ;
#10882 = CARTESIAN_POINT ( 'NONE',  ( 43.01140435219951286, 74.96049967264873715, 29.21067981925356705 ) ) ;
#10883 = CARTESIAN_POINT ( 'NONE',  ( 12.03843011909301453, 134.4860913190374561, 2.577281550626734141 ) ) ;
#10884 = CARTESIAN_POINT ( 'NONE',  ( 58.92189266798492042, 143.1894642327317513, 11.58510527907202992 ) ) ;
#10885 = CARTESIAN_POINT ( 'NONE',  ( -151.4692556286852891, -196.9891397928655010, 49.65701158161630957 ) ) ;
#10886 = CARTESIAN_POINT ( 'NONE',  ( 46.59305225739526435, 77.17977050742732104, 31.60846029578754468 ) ) ;
#10887 = EDGE_LOOP ( 'NONE', ( #6750, #18654, #17968, #18311 ) ) ;
#10888 = ORIENTED_EDGE ( 'NONE', *, *, #8038, .F. ) ;
#10889 = CARTESIAN_POINT ( 'NONE',  ( 47.43856463449117200, 151.7297705074273324, 35.64915139335016647 ) ) ;
#10890 = FACE_OUTER_BOUND ( 'NONE', #13427, .T. ) ;
#10891 = CARTESIAN_POINT ( 'NONE',  ( 48.01140435219951996, 122.2104996726487371, 34.21067981925357060 ) ) ;
#10893 = CARTESIAN_POINT ( 'NONE',  ( 25.37887452999470028, 90.65668055682171200, 1.938985092122112563 ) ) ;
#10892 = CARTESIAN_POINT ( 'NONE',  ( 45.74753988029933538, 74.06518717409399244, 30.44471234641811819 ) ) ;
#10894 = CARTESIAN_POINT ( 'NONE',  ( -142.0420953463935803, -168.5438272943107165, 52.72008163687743831 ) ) ;
#10895 = CARTESIAN_POINT ( 'NONE',  ( 14.48810111090402941, 100.9784058478479523, 15.43442115621699529 ) ) ;
#10896 = CARTESIAN_POINT ( 'NONE',  ( -154.5594255724347761, -183.9630981290893033, 59.16757674456785310 ) ) ;
#10897 = DIRECTION ( 'NONE',  ( 1.000000000000000000, 0.000000000000000000, 0.000000000000000000 ) ) ;
#10898 = CARTESIAN_POINT ( 'NONE',  ( 48.01140435219951996, 157.2844580088725763, 34.21067981925357060 ) ) ;
#10899 = CARTESIAN_POINT ( 'NONE',  ( 43.01140435219951286, 145.1297705074273097, 38.86567161673127657 ) ) ;
#10900 = CARTESIAN_POINT ( 'NONE',  ( 73.37616494982036386, 135.8902282719419077, 4.049127002338204662 ) ) ;
#10901 = CARTESIAN_POINT ( 'NONE',  ( 41.64333658814960870, 128.5151871740939953, 30.00020018409699318 ) ) ;
#10902 = CARTESIAN_POINT ( 'NONE',  ( 43.80332655382220253, 136.5373810949690210, 39.21067981925355639 ) ) ;
#10903 = CARTESIAN_POINT ( 'NONE',  ( -143.8425227516148084, -168.3584106276440480, 44.11586579668791330 ) ) ;
#10904 = AXIS2_PLACEMENT_3D ( 'NONE', #10000, #13617, #16922 ) ;
#10905 = DIRECTION ( 'NONE',  ( 0.000000000000000000, 0.000000000000000000, 1.000000000000000000 ) ) ;
#10906 = DIRECTION ( 'NONE',  ( -0.5010362705417045204, -0.000000000000000000, 0.8654262854811263228 ) ) ;
#10907 = CARTESIAN_POINT ( 'NONE',  ( 62.98455118117477980, 139.9299249275418617, 10.79496628861178387 ) ) ;
#10908 = CARTESIAN_POINT ( 'NONE',  ( 41.46631938032478359, 121.3104996726487457, 38.96596240072933170 ) ) ;
#10909 = CARTESIAN_POINT ( 'NONE',  ( 40.27526882409969033, 102.5651871740939782, 37.97664729208901946 ) ) ;
#10910 = ORIENTED_EDGE ( 'NONE', *, *, #6268, .F. ) ;
#10911 = CARTESIAN_POINT ( 'NONE',  ( 33.01140435219951286, 119.9070776186055838, -35.00000000000000000 ) ) ;
#10912 = VERTEX_POINT ( 'NONE', #8321 ) ;
#10913 = CARTESIAN_POINT ( 'NONE',  ( 44.55648932407425633, 93.68445800887258201, 38.96596240072933170 ) ) ;
#10914 = CARTESIAN_POINT ( 'NONE',  ( 48.01140435219951996, 149.3604996726487286, 32.58608133808903773 ) ) ;
#10916 = CARTESIAN_POINT ( 'NONE',  ( 15.42009695863806229, 114.4785911120537634, -4.053384917639696994 ) ) ;
#10915 = CARTESIAN_POINT ( 'NONE',  ( 47.43856463449118621, 109.6151871740940038, 34.21067981925357060 ) ) ;
#10917 = CARTESIAN_POINT ( 'NONE',  ( 45.51148226160370314, 59.71123016864975597, 29.88059778228138441 ) ) ;
#10919 = CARTESIAN_POINT ( 'NONE',  ( 43.01140435219951286, 95.03445800887257633, 29.21067981925356705 ) ) ;
#10918 = CYLINDRICAL_SURFACE ( 'NONE', #14677, 7.500000000000000000 ) ;
#10920 = CARTESIAN_POINT ( 'NONE',  ( -154.5594255724347761, -186.9630981290893033, 59.16757674456785310 ) ) ;
#10921 = CARTESIAN_POINT ( 'NONE',  ( 43.01140435219951996, 10.71049967264875491, 29.21067981925357060 ) ) ;
#10922 = CARTESIAN_POINT ( 'NONE',  ( 43.01140435219951286, 66.86518717409397539, 38.86567161673127657 ) ) ;
#10923 = CARTESIAN_POINT ( 'NONE',  ( 20.75180444880664510, 93.89949152720284076, -5.875022464008872625 ) ) ;
#10924 = CARTESIAN_POINT ( 'NONE',  ( 41.46631938032478359, 63.11049967264874283, 29.45539723777780239 ) ) ;
#10925 = CARTESIAN_POINT ( 'NONE',  ( -157.2955611005346270, -172.4438272943107506, 57.67623309621198047 ) ) ;
#10926 = ORIENTED_EDGE ( 'NONE', *, *, #20650, .T. ) ;
#10927 = CARTESIAN_POINT ( 'NONE',  ( -145.6429501568359797, -181.1084106276440195, 57.67623309621198047 ) ) ;
#10928 = CARTESIAN_POINT ( 'NONE',  ( 18.00183652574411397, 143.4013020786237860, 8.929911949387623338 ) ) ;
#10929 = FILL_AREA_STYLE ('',( #4201 ) ) ;
#10930 = CARTESIAN_POINT ( 'NONE',  ( 38.58424406990786082, 132.1151871740940180, 34.21067981925357060 ) ) ;
#10931 = MECHANICAL_DESIGN_GEOMETRIC_PRESENTATION_REPRESENTATION (  '', ( #15142 ), #16546 ) ;
#10932 = CARTESIAN_POINT ( 'NONE',  ( 45.74753988029934249, 100.4297705074273210, 37.97664729208901235 ) ) ;
#10933 = EDGE_LOOP ( 'NONE', ( #5446, #16391, #17909, #7957, #18415, #7988 ) ) ;
#10934 = ORIENTED_EDGE ( 'NONE', *, *, #1181, .F. ) ;
#10935 = CARTESIAN_POINT ( 'NONE',  ( 38.24087231542673493, 147.7000375650850970, 3.727681574521009900 ) ) ;
#10936 = EDGE_CURVE ( 'NONE', #1013, #12255, #17110, .T. ) ;
#10937 = ORIENTED_EDGE ( 'NONE', *, *, #18933, .F. ) ;
#10938 = CARTESIAN_POINT ( 'NONE',  ( 44.55648932407425633, 112.8844580088725849, 29.45539723777780239 ) ) ;
#10939 = CARTESIAN_POINT ( 'NONE',  ( 43.01140435219951286, 74.96049967264873715, 29.21067981925356705 ) ) ;
#10940 = CARTESIAN_POINT ( 'NONE',  ( 40.27526882409969033, 132.5651871740940067, 37.97664729208901946 ) ) ;
#10941 =( BOUNDED_CURVE ( )  B_SPLINE_CURVE ( 2, ( #6798, #5130, #11849, #18578, #10208, #8770, #16911 ),
 .UNSPECIFIED., .F., .F. ) 
 B_SPLINE_CURVE_WITH_KNOTS ( ( 3, 2, 2, 3 ),
 ( 0.000000000000000000, 0.007142857142857142634, 0.01428571428571428527, 0.01785714285714286656 ),
 .UNSPECIFIED. ) 
 CURVE ( )  GEOMETRIC_REPRESENTATION_ITEM ( )  RATIONAL_B_SPLINE_CURVE ( ( 1.000000000000000000, 0.9510565162951535312, 1.000000000000000000, 0.9510565162951535312, 1.000000000000000000, 0.9755282581475767101, 0.9755282581475768211 ) ) 
 REPRESENTATION_ITEM ( '' )  );
#10942 = CARTESIAN_POINT ( 'NONE',  ( 46.10157429594899270, 89.66049967264873999, 29.95742577749337343 ) ) ;
#10943 = CARTESIAN_POINT ( 'NONE',  ( 53.71239221804358976, 87.38980250447106357, 6.982120393166105998 ) ) ;
#10944 = CIRCLE ( 'NONE', #8130, 24.99999999999999289 ) ;
#10945 = DIRECTION ( 'NONE',  ( 0.000000000000000000, -1.000000000000000000, 0.000000000000000000 ) ) ;
#10946 = CARTESIAN_POINT ( 'NONE',  ( -141.4692556286852891, -160.1391397928654499, 52.90620854394536821 ) ) ;
#10947 = CARTESIAN_POINT ( 'NONE',  ( 47.05648932407426344, 157.9104996726487400, 37.14960608071593384 ) ) ;
#10948 = CARTESIAN_POINT ( 'NONE',  ( 41.46631938032478359, 144.3844580088725991, 38.96596240072933170 ) ) ;
#10949 = DIRECTION ( 'NONE',  ( 0.4999999999999996114, 0.000000000000000000, 0.8660254037844388186 ) ) ;
#10950 = ORIENTED_EDGE ( 'NONE', *, *, #19450, .F. ) ;
#10951 = CARTESIAN_POINT ( 'NONE',  ( 40.27526882409969033, 71.92977050742729261, 30.44471234641811819 ) ) ;
#10952 = CARTESIAN_POINT ( 'NONE',  ( -142.0420953463935803, -162.5438272943106881, 52.72008163687743831 ) ) ;
#10953 = CARTESIAN_POINT ( 'NONE',  ( 40.73010619540765020, 85.74955863377461185, -6.589596535617429751 ) ) ;
#10954 = DIRECTION ( 'NONE',  ( 0.8660400450101282122, -5.766140419743141397E-05, -0.4999746364707088886 ) ) ;
#10955 = ORIENTED_EDGE ( 'NONE', *, *, #1543, .F. ) ;
#10956 = CARTESIAN_POINT ( 'NONE',  ( 42.21948215057684450, 118.3836182503284675, 39.21067981925355639 ) ) ;
#10957 = CARTESIAN_POINT ( 'NONE',  ( 147.8787791192428074, -126.9891397928655010, 0.3429884183836981459 ) ) ;
#10958 = CARTESIAN_POINT ( 'NONE',  ( 41.64333658814960870, 135.9797705074273324, 38.42115945441014446 ) ) ;
#10959 = VERTEX_POINT ( 'NONE', #10705 ) ;
#10960 = CARTESIAN_POINT ( 'NONE',  ( -151.4692556286852891, -196.9891397928655010, 49.65701158161630957 ) ) ;
#10961 = ORIENTED_EDGE ( 'NONE', *, *, #15712, .F. ) ;
#10962 = CARTESIAN_POINT ( 'NONE',  ( 38.58424406990784661, 123.2297705074273040, 32.77220824515698183 ) ) ;
#10963 = EDGE_CURVE ( 'NONE', #1853, #13715, #17408, .T. ) ;
#10964 = CIRCLE ( 'NONE', #6774, 9.000000000000007105 ) ;
#10965 = CARTESIAN_POINT ( 'NONE',  ( 76.17254549292280785, -61.68114226949890622, 20.00000000000001776 ) ) ;
#10966 = CARTESIAN_POINT ( 'NONE',  ( -159.5594255724347761, -191.1891397928654897, 55.53486410454104316 ) ) ;
#10967 = EDGE_CURVE ( 'NONE', #19975, #4691, #6676, .T. ) ;
#10968 = DIRECTION ( 'NONE',  ( 0.000000000000000000, 0.000000000000000000, 1.000000000000000000 ) ) ;
#10969 = CARTESIAN_POINT ( 'NONE',  ( -151.4692556286852891, -162.8130981290893260, 60.17163382399899518 ) ) ;
#10970 = SHAPE_DEFINITION_REPRESENTATION ( #21701, #6206 ) ;
#10971 = CARTESIAN_POINT ( 'NONE',  ( 44.55648932407425633, 132.6844580088725820, 38.96596240072933170 ) ) ;
#10972 = CARTESIAN_POINT ( 'NONE',  ( 40.27526882409969033, 113.9297705074273068, 30.44471234641811819 ) ) ;
#10973 = CARTESIAN_POINT ( 'NONE',  ( 58.30185729850432352, 143.6975816885063750, 10.55682690296339032 ) ) ;
#10974 = CARTESIAN_POINT ( 'NONE',  ( -154.3824083646099439, -188.4938272943107336, 40.69124936498395328 ) ) ;
#10975 = CARTESIAN_POINT ( 'NONE',  ( 44.37947211624943833, 95.21518717409399812, 30.00020018409699318 ) ) ;
#10976 = CARTESIAN_POINT ( 'NONE',  ( 39.92123440845005433, 90.26049967264873430, 29.95742577749336988 ) ) ;
#10977 = ORIENTED_EDGE ( 'NONE', *, *, #1438, .T. ) ;
#10978 = CARTESIAN_POINT ( 'NONE',  ( 38.01140435219952707, 87.71049967264873715, 34.21067981925357060 ) ) ;
#10979 = CARTESIAN_POINT ( 'NONE',  ( 9.656473946750173454, 127.6128973189080398, 2.339233609801092406 ) ) ;
#10980 = CARTESIAN_POINT ( 'NONE',  ( 49.21618705061847265, 147.3337112213800140, -15.83906960951095577 ) ) ;
#10981 = PRODUCT_DEFINITION_SHAPE ( 'NONE', 'NONE',  #21819 ) ;
#10982 = CARTESIAN_POINT ( 'NONE',  ( -145.2889157411863437, -169.4391397928654328, 58.16351966513671812 ) ) ;
#10983 = VECTOR ( 'NONE', #8649, 1000.000000000000000 ) ;
#10984 = CARTESIAN_POINT ( 'NONE',  ( 46.59305225739526435, 74.17977050742732104, 31.60846029578754468 ) ) ;
#10985 = VERTEX_POINT ( 'NONE', #5621 ) ;
#10986 = EDGE_LOOP ( 'NONE', ( #1689, #1010, #874, #18746 ) ) ;
#10987 = CARTESIAN_POINT ( 'NONE',  ( 45.74753988029933538, 158.3297705074273267, 30.44471234641811819 ) ) ;
#10988 = AXIS2_PLACEMENT_3D ( 'NONE', #12188, #20688, #82 ) ;
#10989 = CARTESIAN_POINT ( 'NONE',  ( 96.62434152388762243, 220.7958015105191976, -5.999999999999976019 ) ) ;
#10990 = CARTESIAN_POINT ( 'NONE',  ( 38.96631938032478359, 123.4104996726487542, 31.27175355779120025 ) ) ;
#10992 = CARTESIAN_POINT ( 'NONE',  ( 57.55288598684787615, 89.00415807515548750, -6.156345639627279986 ) ) ;
#10991 = CARTESIAN_POINT ( 'NONE',  ( 43.01140435219951286, 81.86518717409398960, 38.86567161673127657 ) ) ;
#10993 = CARTESIAN_POINT ( 'NONE',  ( -143.8425227516148084, -168.0938272943107563, 44.11586579668791330 ) ) ;
#10994 = CARTESIAN_POINT ( 'NONE',  ( 52.46025766099742071, 152.8098426157893925, 11.14871012209260748 ) ) ;
#10995 = CARTESIAN_POINT ( 'NONE',  ( -157.6495955161842062, -191.0130981290893146, 41.15050349809590102 ) ) ;
#10996 = LINE ( 'NONE', #17601, #20589 ) ;
#10997 = DIRECTION ( 'NONE',  ( -0.8695660798558993987, -0.4938165983075534782, 0.000000000000000000 ) ) ;
#10998 = CARTESIAN_POINT ( 'NONE',  ( 47.43856463449117200, 146.0297705074272869, 32.77220824515698183 ) ) ;
#10999 = CARTESIAN_POINT ( 'NONE',  ( 36.32848368193762667, 153.5644447507555981, 2.620555573812929584 ) ) ;
#11000 = CARTESIAN_POINT ( 'NONE',  ( 38.58424406990785371, 126.2651871740940237, 35.64915139335015937 ) ) ;
#11001 = CARTESIAN_POINT ( 'NONE',  ( 38.01140435219952707, 69.86049967264871441, 35.83527830041809636 ) ) ;
#11002 = CARTESIAN_POINT ( 'NONE',  ( -143.8425227516148084, -156.9584106276440423, 55.19815736654470584 ) ) ;
#11003 = FACE_OUTER_BOUND ( 'NONE', #11770, .T. ) ;
#11004 = DIRECTION ( 'NONE',  ( 0.000000000000000000, 1.000000000000000000, 0.000000000000000000 ) ) ;
#11005 = CARTESIAN_POINT ( 'NONE',  ( 44.65913741311992879, 148.1402468479653578, 16.98531508000710843 ) ) ;
#11006 = CARTESIAN_POINT ( 'NONE',  ( 39.42975644700377558, 105.4151871740940152, 36.81289934271958941 ) ) ;
#11007 = ORIENTED_EDGE ( 'NONE', *, *, #4516, .F. ) ;
#11008 = EDGE_CURVE ( 'NONE', #1334, #10633, #13385, .T. ) ;
#11009 = DIRECTION ( 'NONE',  ( -0.000000000000000000, -0.000000000000000000, -1.000000000000000000 ) ) ;
#11010 = VERTEX_POINT ( 'NONE', #20625 ) ;
#11011 = CARTESIAN_POINT ( 'NONE',  ( 38.96631938032478359, 92.48445800887257917, 31.27175355779120025 ) ) ;
#11012 = DIRECTION ( 'NONE',  ( 1.000000000000000000, 0.000000000000000000, -0.000000000000000000 ) ) ;
#11013 = CARTESIAN_POINT ( 'NONE',  ( 48.01140435219951996, 152.0604996726487457, 35.83527830041810347 ) ) ;
#11015 = CARTESIAN_POINT ( 'NONE',  ( 68.06566224877710169, 132.6756899087416457, -7.863043133634088910 ) ) ;
#11014 = CARTESIAN_POINT ( 'NONE',  ( 38.58424406990784661, 107.9651871740939839, 32.77220824515698183 ) ) ;
#11016 = CARTESIAN_POINT ( 'NONE',  ( 41.46631938032478359, 67.31049967264873146, 38.96596240072933170 ) ) ;
#11018 = CARTESIAN_POINT ( 'NONE',  ( 46.10157429594899270, 60.83445800887256638, 38.46393386101375711 ) ) ;
#11017 = CARTESIAN_POINT ( 'NONE',  ( 43.01140435219952707, 144.9070776186055696, 39.21067981925356349 ) ) ;
#11019 = CYLINDRICAL_SURFACE ( 'NONE', #5554, 4.999999999999997335 ) ;
#11020 = CARTESIAN_POINT ( 'NONE',  ( -153.0531000319306543, -188.2362167067690848, 39.65701158161630246 ) ) ;
#11021 = DIRECTION ( 'NONE',  ( -0.000000000000000000, 1.000000000000000000, -0.000000000000000000 ) ) ;
#11022 = CARTESIAN_POINT ( 'NONE',  ( 8.944919112598912037, 123.2842988173194385, -4.803623532975393573 ) ) ;
#11023 = CARTESIAN_POINT ( 'NONE',  ( 43.01140435219951996, 10.71049967264875491, 29.21067981925357060 ) ) ;
#11024 = CARTESIAN_POINT ( 'NONE',  ( -160.8964159109769696, -169.7438272943106767, 52.72008163687743121 ) ) ;
#11025 = CARTESIAN_POINT ( 'NONE',  ( -157.2955611005345986, -185.6084106276440195, 41.63779006702063867 ) ) ;
#11026 = ORIENTED_EDGE ( 'NONE', *, *, #2682, .F. ) ;
#11027 = CARTESIAN_POINT ( 'NONE',  ( -151.4692556286852891, -169.4084106276440593, 59.56931450028537967 ) ) ;
#11028 = CARTESIAN_POINT ( 'NONE',  ( 73.49404125747247463, 104.1488224428393039, 5.120290292223307560 ) ) ;
#11029 = EDGE_LOOP ( 'NONE', ( #1093, #14471, #17991, #11197 ) ) ;
#11030 = CARTESIAN_POINT ( 'NONE',  ( 44.37947211624943833, 136.0151871740939953, 38.42115945441014446 ) ) ;
#11031 = CARTESIAN_POINT ( 'NONE',  ( 38.58424406990785371, 93.52977050742731535, 35.64915139335015937 ) ) ;
#11032 = EDGE_LOOP ( 'NONE', ( #13025, #12274, #17229, #10934 ) ) ;
#11033 = ORIENTED_EDGE ( 'NONE', *, *, #882, .F. ) ;
#11034 = CARTESIAN_POINT ( 'NONE',  ( 33.01799438418878907, 146.2770090272405810, 10.51364782838779099 ) ) ;
#11035 = EDGE_LOOP ( 'NONE', ( #13073, #11354, #5547, #9939 ) ) ;
#11036 = CARTESIAN_POINT ( 'NONE',  ( 38.01140435219951996, 113.9344580088725820, 35.83527830041810347 ) ) ;
#11037 = DIRECTION ( 'NONE',  ( 0.000000000000000000, 1.000000000000000000, 0.000000000000000000 ) ) ;
#11038 = CARTESIAN_POINT ( 'NONE',  ( 40.27526882409969033, 72.82977050742732672, 37.97664729208901946 ) ) ;
#11039 = CARTESIAN_POINT ( 'NONE',  ( 39.42975644700377558, 134.8151871740940067, 31.60846029578754468 ) ) ;
#11040 = CARTESIAN_POINT ( 'NONE',  ( 38.01140435219952707, 90.71049967264873715, 34.21067981925357060 ) ) ;
#11041 = CARTESIAN_POINT ( 'NONE',  ( 57.14511974427749408, 88.72838517433189054, 6.862995836283489304 ) ) ;
#11042 = CARTESIAN_POINT ( 'NONE',  ( 38.67454084765554256, 95.28543445581169635, 31.70117790783977796 ) ) ;
#11043 = CARTESIAN_POINT ( 'NONE',  ( -159.5594255724347761, -161.7891397928654555, 43.77915905869157598 ) ) ;
#11044 = CARTESIAN_POINT ( 'NONE',  ( -143.3790856849358306, -158.7630981290893146, 43.77915905869157598 ) ) ;
#11045 = UNCERTAINTY_MEASURE_WITH_UNIT (LENGTH_MEASURE( 1.000000000000000082E-05 ), #21064, 'distance_accuracy_value', 'NONE');
#11046 = CARTESIAN_POINT ( 'NONE',  ( 43.01140435219951996, 10.71049967264875491, 39.21067981925356349 ) ) ;
#11047 = FACE_OUTER_BOUND ( 'NONE', #15907, .T. ) ;
#11048 = ORIENTED_EDGE ( 'NONE', *, *, #1822, .F. ) ;
#11049 = CARTESIAN_POINT ( 'NONE',  ( 43.01140435219951286, 73.12977050742729546, 38.86567161673127657 ) ) ;
#11050 = CARTESIAN_POINT ( 'NONE',  ( -160.8964159109769696, -163.7438272943107336, 52.72008163687743121 ) ) ;
#11051 = CARTESIAN_POINT ( 'NONE',  ( 36.55618291757107841, 153.5264344809625641, -3.375052104409746789 ) ) ;
#11052 = DIRECTION ( 'NONE',  ( -1.000000000000000000, 0.000000000000000000, 0.000000000000000000 ) ) ;
#11053 = ORIENTED_EDGE ( 'NONE', *, *, #14612, .T. ) ;
#11054 = DIRECTION ( 'NONE',  ( -0.9385982292947088190, -0.3450121214752274179, 0.000000000000000000 ) ) ;
#11055 = AXIS2_PLACEMENT_3D ( 'NONE', #14405, #5708, #751 ) ;
#11056 = CARTESIAN_POINT ( 'NONE',  ( 41.64333658814960870, 126.9797705074273182, 38.42115945441014446 ) ) ;
#11057 = ORIENTED_EDGE ( 'NONE', *, *, #10694, .F. ) ;
#11058 = CARTESIAN_POINT ( 'NONE',  ( 43.80332655382220253, 87.61133943119283174, 39.21067981925355639 ) ) ;
#11059 =( BOUNDED_CURVE ( )  B_SPLINE_CURVE ( 2, ( #823, #17568, #9316, #501, #15594, #16018, #17458, #15806, #11065, #930, #14372, #7675, #12508 ),
 .UNSPECIFIED., .F., .F. ) 
 B_SPLINE_CURVE_WITH_KNOTS ( ( 3, 2, 2, 2, 2, 2, 3 ),
 ( 0.5808823529411765163, 0.5823529411764706287, 0.5852941176470588536, 0.5882352941176470784, 0.5911764705882353033, 0.5941176470588235281, 0.5955882352941176405 ),
 .UNSPECIFIED. ) 
 CURVE ( )  GEOMETRIC_REPRESENTATION_ITEM ( )  RATIONAL_B_SPLINE_CURVE ( ( 0.9755282581475768211, 0.9755282581475768211, 1.000000000000000000, 0.9510565162951535312, 1.000000000000000000, 0.9510565162951535312, 1.000000000000000000, 0.9510565162951535312, 1.000000000000000000, 0.9510565162951535312, 1.000000000000000000, 0.9755282581475768211, 0.9755282581475768211 ) ) 
 REPRESENTATION_ITEM ( '' )  );
#11060 = ORIENTED_EDGE ( 'NONE', *, *, #18850, .F. ) ;
#11061 = CARTESIAN_POINT ( 'NONE',  ( 46.59305225739526435, 122.1797705074273210, 31.60846029578754468 ) ) ;
#11062 = CARTESIAN_POINT ( 'NONE',  ( 44.55648932407425633, 139.8844580088725991, 29.45539723777780239 ) ) ;
#11063 = CARTESIAN_POINT ( 'NONE',  ( 38.01140435219951996, 59.93445800887258912, 35.83527830041810347 ) ) ;
#11064 = EDGE_CURVE ( 'NONE', #6320, #12307, #348, .T. ) ;
#11065 = CARTESIAN_POINT ( 'NONE',  ( 38.96631938032478359, 99.41049967264873999, 31.27175355779120025 ) ) ;
#11066 = CARTESIAN_POINT ( 'NONE',  ( 42.21948215057684450, 83.11133943119283174, 29.21067981925356705 ) ) ;
#11067 = DIRECTION ( 'NONE',  ( -0.000000000000000000, -0.000000000000000000, 1.000000000000000000 ) ) ;
#11068 = CARTESIAN_POINT ( 'NONE',  ( -145.2889157411863721, -186.5391397928654271, 41.15050349809590102 ) ) ;
#11069 = CIRCLE ( 'NONE', #1581, 7.500000000000007105 ) ;
#11070 = CARTESIAN_POINT ( 'NONE',  ( 47.05648932407426344, 125.5104996726487343, 31.27175355779120025 ) ) ;
#11071 = PRODUCT_DEFINITION ( 'UNKNOWN', '', #13384, #13252 ) ;
#11072 = CARTESIAN_POINT ( 'NONE',  ( -141.4692556286852891, -162.0630981290892976, 49.65701158161630957 ) ) ;
#11073 = CARTESIAN_POINT ( 'NONE',  ( 41.46631938032478359, 135.3844580088725706, 38.96596240072933170 ) ) ;
#11074 = CARTESIAN_POINT ( 'NONE',  ( 38.58424406990786082, 105.3797705074273239, 34.21067981925357060 ) ) ;
#11075 = CARTESIAN_POINT ( 'NONE',  ( 68.27453032555700929, 132.6178071945132046, 11.15186410612756696 ) ) ;
#11076 = CARTESIAN_POINT ( 'NONE',  ( -145.6429501568359797, -194.9438272943107222, 41.63779006702063867 ) ) ;
#11077 = CARTESIAN_POINT ( 'NONE',  ( 38.58424406990786082, 96.11518717409400381, 34.21067981925357060 ) ) ;
#11078 = LINE ( 'NONE', #14273, #20911 ) ;
#11079 = VERTEX_POINT ( 'NONE', #19078 ) ;
#11080 = DIRECTION ( 'NONE',  ( 0.000000000000000000, 0.000000000000000000, 1.000000000000000000 ) ) ;
#11081 = EDGE_CURVE ( 'NONE', #8368, #19976, #3705, .T. ) ;
#11082 = CARTESIAN_POINT ( 'NONE',  ( 66.24914683137549787, 94.76885710642066840, 6.506024766557033878 ) ) ;
#11083 = CARTESIAN_POINT ( 'NONE',  ( 71.10646316465144423, 118.7373161137383732, -14.29152813157908319 ) ) ;
#11084 = CARTESIAN_POINT ( 'NONE',  ( 33.56091001181424360, 87.00402361476987778, -6.351118090676544981 ) ) ;
#11085 = CARTESIAN_POINT ( 'NONE',  ( 38.58424406990786082, 75.37977050742732388, 34.21067981925357060 ) ) ;
#11086 = ORIENTED_EDGE ( 'NONE', *, *, #4103, .T. ) ;
#11087 = EDGE_CURVE ( 'NONE', #11247, #20292, #18190, .T. ) ;
#11088 = ORIENTED_EDGE ( 'NONE', *, *, #18399, .T. ) ;
#11089 = CARTESIAN_POINT ( 'NONE',  ( 44.37947211624943833, 151.2797705074273438, 38.42115945441014446 ) ) ;
#11090 = CARTESIAN_POINT ( 'NONE',  ( -55.11860757350579831, 784.8075632535900468, -19.99999999999997868 ) ) ;
#11091 = ADVANCED_FACE ( 'NONE', ( #11228 ), #10918, .F. ) ;
#11092 = AXIS2_PLACEMENT_3D ( 'NONE', #20802, #4046, #17481 ) ;
#11093 = CARTESIAN_POINT ( 'NONE',  ( 38.01140435219951996, 123.8604996726487570, 35.83527830041810347 ) ) ;
#11095 = CARTESIAN_POINT ( 'NONE',  ( 66.03587854725165585, 94.68079322629401418, 0.5104136635535641009 ) ) ;
#11094 = CARTESIAN_POINT ( 'NONE',  ( 39.42975644700377558, 74.81518717409399244, 31.60846029578754468 ) ) ;
#11096 = CARTESIAN_POINT ( 'NONE',  ( 151.4773229304660731, 84.89323405393692212, 14.00000000000001776 ) ) ;
#11097 = CARTESIAN_POINT ( 'NONE',  ( -160.8964159109769696, -170.0438272943107165, 46.59394152635518083 ) ) ;
#11098 = CARTESIAN_POINT ( 'NONE',  ( 77.24268685965694203, 120.2105100216710696, 12.57728155048203433 ) ) ;
#11099 = CARTESIAN_POINT ( 'NONE',  ( -154.5594255724347761, -186.9630981290893033, 59.16757674456785310 ) ) ;
#11100 = CARTESIAN_POINT ( 'NONE',  ( -176.9699209214867324, -126.9891397928655010, -72.64809332337415526 ) ) ;
#11101 = PLANE ( 'NONE',  #1991 ) ;
#11102 = CARTESIAN_POINT ( 'NONE',  ( 38.58424406990786082, 129.3797705074273381, 34.21067981925357060 ) ) ;
#11103 = CARTESIAN_POINT ( 'NONE',  ( 33.74677389505396263, 86.86730044589080535, -0.3555069876874490942 ) ) ;
#11104 = CARTESIAN_POINT ( 'NONE',  ( 47.43856463449118621, 121.6151871740940038, 34.21067981925357060 ) ) ;
#11105 = CARTESIAN_POINT ( 'NONE',  ( 43.01140435219951286, 136.4604996726487514, 39.21067981925356349 ) ) ;
#11106 = CARTESIAN_POINT ( 'NONE',  ( -157.2955611005345986, -160.7084106276440423, 57.67623309621197336 ) ) ;
#11107 = EDGE_CURVE ( 'NONE', #12991, #8122, #8701, .T. ) ;
#11108 = DIRECTION ( 'NONE',  ( 0.000000000000000000, -1.000000000000000000, 0.000000000000000000 ) ) ;
#11109 = CARTESIAN_POINT ( 'NONE',  ( 111.4021762516569964, 137.5714195593754710, 14.00000000000001776 ) ) ;
#11110 = CARTESIAN_POINT ( 'NONE',  ( 20.52669235689029037, 137.0142703344444897, 22.89568392956547882 ) ) ;
#11111 = CIRCLE ( 'NONE', #1613, 5.425037101889737201 ) ;
#11112 = CARTESIAN_POINT ( 'NONE',  ( 44.55648932407425633, 82.61049967264874283, 38.96596240072933170 ) ) ;
#11113 = CARTESIAN_POINT ( 'NONE',  ( 45.74753988029933538, 110.0651871740939782, 30.44471234641811819 ) ) ;
#11114 = EDGE_CURVE ( 'NONE', #15461, #13608, #10119, .T. ) ;
#11115 = ORIENTED_EDGE ( 'NONE', *, *, #9932, .T. ) ;
#11116 = CARTESIAN_POINT ( 'NONE',  ( 43.01140435219951286, 86.96049967264872294, 29.21067981925356705 ) ) ;
#11117 = ORIENTED_EDGE ( 'NONE', *, *, #618, .F. ) ;
#11118 = CARTESIAN_POINT ( 'NONE',  ( 38.01140435219952707, 92.78445800887257633, 34.21067981925357060 ) ) ;
#11119 = FACE_OUTER_BOUND ( 'NONE', #19633, .T. ) ;
#11120 = CARTESIAN_POINT ( 'NONE',  ( 41.46631938032478359, 153.1104996726487570, 29.45539723777780239 ) ) ;
#11122 = CARTESIAN_POINT ( 'NONE',  ( 47.44511438772692458, 147.6747606579048409, -1.910614883896327054 ) ) ;
#11121 = CARTESIAN_POINT ( 'NONE',  ( 38.58424406990786082, 111.1151871740940038, 34.21067981925357060 ) ) ;
#11123 = CARTESIAN_POINT ( 'NONE',  ( 38.96631938032478359, 61.01049967264874141, 37.14960608071593384 ) ) ;
#11125 = CARTESIAN_POINT ( 'NONE',  ( -161.4692556286853176, -157.5630981290892976, 49.65701158161630957 ) ) ;
#11124 = CARTESIAN_POINT ( 'NONE',  ( 46.66402830546390845, 144.6390769119227855, 37.62897400776943613 ) ) ;
#11126 =( NAMED_UNIT ( * ) SI_UNIT ( $, .STERADIAN. ) SOLID_ANGLE_UNIT ( ) );
#11127 = DIRECTION ( 'NONE',  ( -0.000000000000000000, -0.000000000000000000, -1.000000000000000000 ) ) ;
#11128 = CARTESIAN_POINT ( 'NONE',  ( 47.05648932407426344, 146.5104996726487627, 31.27175355779120025 ) ) ;
#11129 = CIRCLE ( 'NONE', #20301, 9.999999999999994671 ) ;
#11130 = CARTESIAN_POINT ( 'NONE',  ( 38.58424406990784661, 69.26518717409398107, 35.64915139335016647 ) ) ;
#11131 = CARTESIAN_POINT ( 'NONE',  ( 13.69124840528610321, 102.2378096837820181, -5.517995706778950016 ) ) ;
#11132 = CARTESIAN_POINT ( 'NONE',  ( -159.0959885057557983, -166.5938272943107563, 55.19815736654470584 ) ) ;
#11133 = CARTESIAN_POINT ( 'NONE',  ( -154.3824083646099439, -185.7584106276440536, 40.69124936498395328 ) ) ;
#11134 = ADVANCED_FACE ( 'NONE', ( #21384 ), #12455, .F. ) ;
#11135 = ORIENTED_EDGE ( 'NONE', *, *, #693, .T. ) ;
#11136 = CARTESIAN_POINT ( 'NONE',  ( -154.3824083646099439, -169.5584106276440366, 58.62277379824867296 ) ) ;
#11137 = CARTESIAN_POINT ( 'NONE',  ( 77.17837728419731036, 116.7372127726149245, 18.69201499742705153 ) ) ;
#11138 =( NAMED_UNIT ( * ) PLANE_ANGLE_UNIT ( ) SI_UNIT ( $, .RADIAN. ) );
#11139 = CARTESIAN_POINT ( 'NONE',  ( 39.42975644700377558, 134.8151871740940067, 31.60846029578754468 ) ) ;
#11140 = VECTOR ( 'NONE', #8494, 1000.000000000000114 ) ;
#11141 = ORIENTED_EDGE ( 'NONE', *, *, #5960, .T. ) ;
#11142 = ORIENTED_EDGE ( 'NONE', *, *, #11781, .T. ) ;
#11143 = CARTESIAN_POINT ( 'NONE',  ( 51.29519266978688563, 92.95216133272363379, 14.08499220319455780 ) ) ;
#11144 = COLOUR_RGB ( '', 0.40784314, 0.44705882, 0.49803922) ;
#11145 = ORIENTED_EDGE ( 'NONE', *, *, #16232, .T. ) ;
#11146 = CARTESIAN_POINT ( 'NONE',  ( 38.01140435219951996, 116.6344580088725564, 32.58608133808903773 ) ) ;
#11147 = DIRECTION ( 'NONE',  ( 0.000000000000000000, 0.000000000000000000, 1.000000000000000000 ) ) ;
#11148 = CARTESIAN_POINT ( 'NONE',  ( 38.58424406990786082, 72.37977050742732388, 34.21067981925357060 ) ) ;
#11149 = CARTESIAN_POINT ( 'NONE',  ( 46.59305225739526435, 139.3151871740940067, 36.81289934271958941 ) ) ;
#11150 = CARTESIAN_POINT ( 'NONE',  ( 48.01140435219951996, 95.21049967264875136, 34.21067981925357060 ) ) ;
#11151 = CARTESIAN_POINT ( 'NONE',  ( 70.26356658872128946, 140.6255928306487704, 11.86290872716119615 ) ) ;
#11152 = DIRECTION ( 'NONE',  ( 0.000000000000000000, 0.000000000000000000, -1.000000000000000000 ) ) ;
#11153 = CARTESIAN_POINT ( 'NONE',  ( -161.4692556286853176, -161.4891397928654726, 49.65701158161630957 ) ) ;
#11154 = VECTOR ( 'NONE', #19549, 1000.000000000000000 ) ;
#11155 = CARTESIAN_POINT ( 'NONE',  ( 54.85617982533816672, 239.2521282348021714, -3.999999999999980904 ) ) ;
#11156 = PRODUCT_DEFINITION_SHAPE ( 'NONE', 'NONE',  #21829 ) ;
#11157 = CARTESIAN_POINT ( 'NONE',  ( -153.0531000319306827, -186.1622583705452030, 39.65701158161629536 ) ) ;
#11158 = ORIENTED_EDGE ( 'NONE', *, *, #19749, .T. ) ;
#11159 = CARTESIAN_POINT ( 'NONE',  ( 38.58424406990786082, 75.37977050742732388, 34.21067981925357060 ) ) ;
#11160 = CARTESIAN_POINT ( 'NONE',  ( -160.8964159109769696, -194.1584106276440593, 49.65701158161630957 ) ) ;
#11161 = CARTESIAN_POINT ( 'NONE',  ( 9.021810916323596885, 123.9851095102452945, 2.220310480865780534 ) ) ;
#11162 = CARTESIAN_POINT ( 'NONE',  ( -151.4692556286852891, -190.4084106276440309, 59.56931450028537967 ) ) ;
#11163 = ORIENTED_EDGE ( 'NONE', *, *, #11087, .F. ) ;
#11164 = CARTESIAN_POINT ( 'NONE',  ( 43.01140435219957681, 97.46049967264875136, 39.21067981925356349 ) ) ;
#11165 = CARTESIAN_POINT ( 'NONE',  ( 44.55648932407425633, 124.8844580088725706, 29.45539723777780239 ) ) ;
#11166 = CARTESIAN_POINT ( 'NONE',  ( 44.37947211624943833, 125.4797705074273182, 30.00020018409699318 ) ) ;
#11167 = EDGE_CURVE ( 'NONE', #20725, #417, #4082, .T. ) ;
#11168 = VECTOR ( 'NONE', #16435, 1000.000000000000000 ) ;
#11169 = EDGE_LOOP ( 'NONE', ( #7822, #20943, #17199, #8860 ) ) ;
#11170 = CARTESIAN_POINT ( 'NONE',  ( 44.55648932407425633, 88.88445800887258486, 29.45539723777780239 ) ) ;
#11171 = ORIENTED_EDGE ( 'NONE', *, *, #17447, .F. ) ;
#11172 = CARTESIAN_POINT ( 'NONE',  ( 44.37947211624943833, 124.2797705074273154, 38.42115945441014446 ) ) ;
#11173 = AXIS2_PLACEMENT_3D ( 'NONE', #13429, #96, #1635 ) ;
#11174 = CARTESIAN_POINT ( 'NONE',  ( 43.01140435219957681, 68.03445800887257633, 29.21067981925356705 ) ) ;
#11175 = CARTESIAN_POINT ( 'NONE',  ( 41.46631938032478359, 68.18445800887256780, 29.45539723777780239 ) ) ;
#11176 = LINE ( 'NONE', #16134, #10464 ) ;
#11177 = CARTESIAN_POINT ( 'NONE',  ( 38.01140435219952707, 101.9344580088725678, 35.83527830041809636 ) ) ;
#11178 = CARTESIAN_POINT ( 'NONE',  ( -161.4692556286852607, -185.3391397928654953, 52.90620854394536821 ) ) ;
#11179 = CARTESIAN_POINT ( 'NONE',  ( 43.01140435219951286, 60.53445800887258343, 39.21067981925356349 ) ) ;
#11180 = CARTESIAN_POINT ( 'NONE',  ( 44.55648932407425633, 130.6104996726487286, 38.96596240072933170 ) ) ;
#11181 = CARTESIAN_POINT ( 'NONE',  ( -148.5561028927606344, -186.9938272943107336, 58.62277379824867296 ) ) ;
#11182 = CIRCLE ( 'NONE', #19638, 5.425037101889737201 ) ;
#11183 = CARTESIAN_POINT ( 'NONE',  ( 46.10157429594899270, 123.8344580088725735, 38.46393386101376421 ) ) ;
#11184 = CARTESIAN_POINT ( 'NONE',  ( 46.59305225739526435, 100.5797705074273267, 36.81289934271958941 ) ) ;
#11185 = CARTESIAN_POINT ( 'NONE',  ( 67.11143925497957241, 134.7062941969633414, 18.05698923925237764 ) ) ;
#11186 = CARTESIAN_POINT ( 'NONE',  ( -142.0420953463936087, -183.3938272943107108, 49.65701158161630957 ) ) ;
#11187 = CARTESIAN_POINT ( 'NONE',  ( 45.74753988029934249, 101.0651871740939924, 30.44471234641812174 ) ) ;
#11188 = CARTESIAN_POINT ( 'NONE',  ( -143.3790856849358306, -161.7630981290893146, 43.77915905869157598 ) ) ;
#11189 = VERTEX_POINT ( 'NONE', #7727 ) ;
#11190 = CARTESIAN_POINT ( 'NONE',  ( 46.10157429594899270, 128.6604996726487400, 29.95742577749336988 ) ) ;
#11191 = ADVANCED_FACE ( 'NONE', ( #4392 ), #12673, .T. ) ;
#11192 = CARTESIAN_POINT ( 'NONE',  ( 37.24990543953586553, 153.6521207556136517, 3.648881909465930828 ) ) ;
#11193 =( BOUNDED_CURVE ( )  B_SPLINE_CURVE ( 2, ( #12413, #2490, #9011, #17583, #5575, #15722, #19143, #16032, #4252, #12633, #7361, #5793, #19354 ),
 .UNSPECIFIED., .F., .T. ) 
 B_SPLINE_CURVE_WITH_KNOTS ( ( 3, 2, 2, 2, 2, 2, 3 ),
 ( 0.8014705882352941568, 0.8029411764705882693, 0.8058823529411764941, 0.8088235294117647189, 0.8117647058823529438, 0.8147058823529411686, 0.8161764705882352811 ),
 .UNSPECIFIED. ) 
 CURVE ( )  GEOMETRIC_REPRESENTATION_ITEM ( )  RATIONAL_B_SPLINE_CURVE ( ( 0.9755282581475768211, 0.9755282581475768211, 1.000000000000000000, 0.9510565162951535312, 1.000000000000000000, 0.9510565162951535312, 1.000000000000000000, 0.9510565162951535312, 1.000000000000000000, 0.9510565162951535312, 1.000000000000000000, 0.9755282581475768211, 0.9755282581475768211 ) ) 
 REPRESENTATION_ITEM ( '' )  );
#11194 = CARTESIAN_POINT ( 'NONE',  ( 25.00529828370466490, 141.4305569644042464, -16.86339438981633876 ) ) ;
#11195 = CARTESIAN_POINT ( 'NONE',  ( 40.27526882409969744, 65.92977050742732104, 30.44471234641812174 ) ) ;
#11196 = ORIENTED_EDGE ( 'NONE', *, *, #20824, .F. ) ;
#11197 = ORIENTED_EDGE ( 'NONE', *, *, #4559, .F. ) ;
#11198 = CARTESIAN_POINT ( 'NONE',  ( 47.43856463449117200, 152.0297705074273438, 32.77220824515698183 ) ) ;
#11199 = CARTESIAN_POINT ( 'NONE',  ( -81.61981105773979550, 604.5992151483073940, -0.8325491102011938205 ) ) ;
#11200 = CARTESIAN_POINT ( 'NONE',  ( 44.55648932407425633, 121.6104996726487570, 38.96596240072933170 ) ) ;
#11202 = CARTESIAN_POINT ( 'NONE',  ( 18.86674891209846905, 143.9013856721611546, -11.04182128657428485 ) ) ;
#11201 = CARTESIAN_POINT ( 'NONE',  ( 46.59305225739526435, 67.91518717409400097, 31.60846029578754468 ) ) ;
#11203 = CARTESIAN_POINT ( 'NONE',  ( -142.0420953463935803, -168.2438272943107336, 46.59394152635518083 ) ) ;
#11204 = CARTESIAN_POINT ( 'NONE',  ( 38.01140435219952707, 155.9344580088725820, 35.83527830041809636 ) ) ;
#11205 = CARTESIAN_POINT ( 'NONE',  ( -159.5594255724347761, -178.8630981290893089, 43.77915905869157598 ) ) ;
#11206 = DIRECTION ( 'NONE',  ( -0.000000000000000000, -0.000000000000000000, -1.000000000000000000 ) ) ;
#11207 = CARTESIAN_POINT ( 'NONE',  ( 41.64333658814960870, 135.9797705074273324, 38.42115945441014446 ) ) ;
#11208 = EDGE_CURVE ( 'NONE', #11408, #14439, #9164, .T. ) ;
#11209 = CARTESIAN_POINT ( 'NONE',  ( 44.63232748576950115, 85.63068390643836381, -0.7129156696548789585 ) ) ;
#11210 = CARTESIAN_POINT ( 'NONE',  ( 43.01140435219951286, 128.3651871740940180, 29.55568802177586107 ) ) ;
#11211 = DIRECTION ( 'NONE',  ( -0.3428981916074306802, 0.9393725726208711491, 0.000000000000000000 ) ) ;
#11212 = CARTESIAN_POINT ( 'NONE',  ( -151.4692556286852891, -158.9084106276440309, 39.74470866294723947 ) ) ;
#11213 = LINE ( 'NONE', #13093, #4490 ) ;
#11214 = CARTESIAN_POINT ( 'NONE',  ( 65.02675087932300357, 102.2843278501921418, -7.581721168364237151 ) ) ;
#11215 = CARTESIAN_POINT ( 'NONE',  ( 43.80332655382220253, 82.53738109496899256, 39.21067981925355639 ) ) ;
#11216 = CARTESIAN_POINT ( 'NONE',  ( 45.74753988029933538, 104.0651871740940067, 30.44471234641811819 ) ) ;
#11217 = ORIENTED_EDGE ( 'NONE', *, *, #14093, .F. ) ;
#11218 = CARTESIAN_POINT ( 'NONE',  ( 43.80332655382220253, 86.88361825032846752, 29.21067981925356705 ) ) ;
#11219 = ORIENTED_EDGE ( 'NONE', *, *, #3557, .F. ) ;
#11220 = CARTESIAN_POINT ( 'NONE',  ( 38.01140435219951996, 86.63445800887255643, 32.58608133808903773 ) ) ;
#11221 = CARTESIAN_POINT ( 'NONE',  ( 57.67197451322198276, 240.2871645992281628, -6.999999999999982236 ) ) ;
#11222 = CARTESIAN_POINT ( 'NONE',  ( 38.96631938032478359, 148.0104996726487627, 37.14960608071593384 ) ) ;
#11224 = CARTESIAN_POINT ( 'NONE',  ( 14.95244176413730131, 118.0514569880088231, 3.089472225200239563 ) ) ;
#11223 = CARTESIAN_POINT ( 'NONE',  ( 46.59305225739526435, 109.9151871740940010, 31.60846029578754468 ) ) ;
#11225 = CARTESIAN_POINT ( 'NONE',  ( -145.6429501568359797, -169.1084106276440480, 57.67623309621198047 ) ) ;
#11226 = CARTESIAN_POINT ( 'NONE',  ( 44.55648932407425633, 62.81049967264873146, 29.45539723777780239 ) ) ;
#11227 = AXIS2_PLACEMENT_3D ( 'NONE', #19836, #3079, #13439 ) ;
#11228 = FACE_OUTER_BOUND ( 'NONE', #15979, .T. ) ;
#11229 = PRESENTATION_STYLE_ASSIGNMENT (( #7835 ) ) ;
#11230 = CARTESIAN_POINT ( 'NONE',  ( 43.01140435219951286, 80.03445800887257633, 29.21067981925356705 ) ) ;
#11231 = CARTESIAN_POINT ( 'NONE',  ( -153.0531000319306543, -189.8899795514095672, 59.65701158161630957 ) ) ;
#11232 = CARTESIAN_POINT ( 'NONE',  ( 39.42975644700377558, 59.81518717409399244, 31.60846029578754468 ) ) ;
#11233 = EDGE_CURVE ( 'NONE', #16997, #20239, #7511, .T. ) ;
#11234 = CARTESIAN_POINT ( 'NONE',  ( 76.20123706073158587, 111.5182621349952257, -8.137091297256032973 ) ) ;
#11235 = CARTESIAN_POINT ( 'NONE',  ( 46.59305225739526435, 151.3151871740940067, 36.81289934271958941 ) ) ;
#11236 = CARTESIAN_POINT ( 'NONE',  ( 43.01140435219951996, 10.71049967264875491, 34.21067981925357060 ) ) ;
#11237 = CARTESIAN_POINT ( 'NONE',  ( -148.5561028927606344, -173.7938272943107165, 40.69124936498395328 ) ) ;
#11238 = CARTESIAN_POINT ( 'NONE',  ( -151.4692556286852891, -182.9084106276440025, 39.74470866294723947 ) ) ;
#11239 = ORIENTED_EDGE ( 'NONE', *, *, #5195, .T. ) ;
#11240 = CARTESIAN_POINT ( 'NONE',  ( 47.43856463449117911, 70.76518717409399528, 32.77220824515697473 ) ) ;
#11241 = CARTESIAN_POINT ( 'NONE',  ( -143.8425227516148084, -165.9584106276440423, 55.19815736654470584 ) ) ;
#11242 = CARTESIAN_POINT ( 'NONE',  ( 31.65106594408818097, 87.52743543124788062, 20.71565594656193454 ) ) ;
#11243 = CARTESIAN_POINT ( 'NONE',  ( 38.58424406990786082, 159.1151871740940180, 34.21067981925357060 ) ) ;
#11244 = CARTESIAN_POINT ( 'NONE',  ( 45.74753988029933538, 137.0651871740940067, 30.44471234641811819 ) ) ;
#11245 = CARTESIAN_POINT ( 'NONE',  ( 64.23777839346797691, 146.6638261710672566, -8.418409733082999225 ) ) ;
#11246 = ORIENTED_EDGE ( 'NONE', *, *, #10032, .T. ) ;
#11247 = VERTEX_POINT ( 'NONE', #19291 ) ;
#11248 = ORIENTED_EDGE ( 'NONE', *, *, #20679, .T. ) ;
#11249 = EDGE_CURVE ( 'NONE', #1447, #7574, #13325, .T. ) ;
#11250 = EDGE_CURVE ( 'NONE', #14746, #7116, #1646, .T. ) ;
#11251 = CARTESIAN_POINT ( 'NONE',  ( 39.42975644700377558, 78.07977050742731251, 31.60846029578754468 ) ) ;
#11252 = CARTESIAN_POINT ( 'NONE',  ( 41.64333658814960870, 135.7151871740940123, 38.42115945441014446 ) ) ;
#11253 = CARTESIAN_POINT ( 'NONE',  ( 38.96631938032478359, 90.41049967264875420, 31.27175355779120025 ) ) ;
#11254 = CARTESIAN_POINT ( 'NONE',  ( 10.91571581598819662, 131.8149664739095783, 9.482090752819161139 ) ) ;
#11255 = CARTESIAN_POINT ( 'NONE',  ( 40.94616811940298362, 94.99207055061751248, 29.65421901078122602 ) ) ;
#11256 = CARTESIAN_POINT ( 'NONE',  ( -157.6495955161842062, -164.9391397928654612, 41.15050349809590102 ) ) ;
#11257 = CARTESIAN_POINT ( 'NONE',  ( 38.58424406990786082, 87.11518717409400381, 34.21067981925357060 ) ) ;
#11258 = DIRECTION ( 'NONE',  ( 0.5061580162706794672, 0.8624407588727068807, 0.000000000000000000 ) ) ;
#11259 = DIRECTION ( 'NONE',  ( 0.000000000000000000, 0.000000000000000000, 1.000000000000000000 ) ) ;
#11260 = CARTESIAN_POINT ( 'NONE',  ( 43.80332655382220253, 61.53738109496899966, 39.21067981925355639 ) ) ;
#11261 = CLOSED_SHELL ( 'NONE', ( #4488, #11359, #8826, #14936, #14195, #11636, #20480, #4593, #8797 ) ) ;
#11262 = CARTESIAN_POINT ( 'NONE',  ( -81.61981105773979550, 604.5992151483073940, -23.16745088979876499 ) ) ;
#11263 = ORIENTED_EDGE ( 'NONE', *, *, #7494, .T. ) ;
#11264 = CARTESIAN_POINT ( 'NONE',  ( 40.27526882409969033, 74.92977050742732104, 30.44471234641811819 ) ) ;
#11265 = CARTESIAN_POINT ( 'NONE',  ( -160.8964159109769696, -194.3084106276440366, 46.59394152635518793 ) ) ;
#11266 = CARTESIAN_POINT ( 'NONE',  ( 32.14050509837299785, 87.44534670509604268, 7.696117750009315195 ) ) ;
#11267 = CARTESIAN_POINT ( 'NONE',  ( -142.0420953463936087, -183.6584106276440309, 49.65701158161630957 ) ) ;
#11268 = ORIENTED_EDGE ( 'NONE', *, *, #3229, .T. ) ;
#11269 = CARTESIAN_POINT ( 'NONE',  ( -39.63192160874135084, -37.13255853780189852, 20.00000000000002132 ) ) ;
#11270 = CARTESIAN_POINT ( 'NONE',  ( 41.46631938032478359, 104.1844580088725820, 29.45539723777780239 ) ) ;
#11271 = CARTESIAN_POINT ( 'NONE',  ( 46.59305225739526435, 122.1797705074273210, 31.60846029578754468 ) ) ;
#11272 = ORIENTED_EDGE ( 'NONE', *, *, #14155, .T. ) ;
#11273 = SURFACE_STYLE_FILL_AREA ( #19661 ) ;
#11274 = VERTEX_POINT ( 'NONE', #18170 ) ;
#11275 = CARTESIAN_POINT ( 'NONE',  ( 41.64333658814960870, 126.9797705074273182, 38.42115945441014446 ) ) ;
#11276 = CARTESIAN_POINT ( 'NONE',  ( -156.4692864601533131, -155.0638355923473455, 40.99677534440144200 ) ) ;
#11277 = CIRCLE ( 'NONE', #2489, 7.500000000000007105 ) ;
#11278 = EDGE_CURVE ( 'NONE', #5881, #20985, #5721, .T. ) ;
#11279 = CARTESIAN_POINT ( 'NONE',  ( 45.74753988029933538, 89.32977050742732672, 30.44471234641811819 ) ) ;
#11280 = CARTESIAN_POINT ( 'NONE',  ( 48.01140435219951996, 64.43445800887258201, 32.58608133808903773 ) ) ;
#11281 = CARTESIAN_POINT ( 'NONE',  ( 161.4980277546683283, 196.8248625098966897, 21.73429951086134082 ) ) ;
#11282 = CARTESIAN_POINT ( 'NONE',  ( 38.96631938032478359, 102.0844580088725877, 37.14960608071593384 ) ) ;
#11283 = FILL_AREA_STYLE_COLOUR ( '', #7398 ) ;
#11284 = CARTESIAN_POINT ( 'NONE',  ( -148.3790856849358306, -193.5891397928654669, 59.16757674456786020 ) ) ;
#11285 = LINE ( 'NONE', #21332, #17506 ) ;
#11286 = CARTESIAN_POINT ( 'NONE',  ( 38.96631938032478359, 103.0104996726487485, 37.14960608071593384 ) ) ;
#11287 = CARTESIAN_POINT ( 'NONE',  ( -148.5561028927606344, -192.9938272943107336, 58.62277379824867296 ) ) ;
#11288 = SHAPE_DEFINITION_REPRESENTATION ( #16260, #21416 ) ;
#11289 = CARTESIAN_POINT ( 'NONE',  ( 44.55648932407425633, 120.6844580088725962, 38.96596240072933170 ) ) ;
#11290 = CARTESIAN_POINT ( 'NONE',  ( 41.64333658814960870, 107.7797705074273154, 30.00020018409699318 ) ) ;
#11291 = CARTESIAN_POINT ( 'NONE',  ( 70.00144543033923128, 111.4600545017090241, 19.00928056007509070 ) ) ;
#11292 = CARTESIAN_POINT ( 'NONE',  ( 43.01140435219951286, 101.3651871740940038, 29.55568802177586107 ) ) ;
#11293 = LINE ( 'NONE', #2926, #15056 ) ;
#11294 = ORIENTED_EDGE ( 'NONE', *, *, #4303, .F. ) ;
#11295 = CARTESIAN_POINT ( 'NONE',  ( 141.4773229304660447, 84.89323405393692212, -19.99999999999997868 ) ) ;
#11296 = CARTESIAN_POINT ( 'NONE',  ( 13.33420504782278293, 102.8437529505761603, 1.505736668420971869 ) ) ;
#11297 = CARTESIAN_POINT ( 'NONE',  ( 57.54249972904700172, 143.9818934734506115, -15.48196187774845356 ) ) ;
#11298 = CARTESIAN_POINT ( 'NONE',  ( 41.64333658814960870, 69.97977050742731819, 38.42115945441014446 ) ) ;
#11299 = VERTEX_POINT ( 'NONE', #6271 ) ;
#11300 = ORIENTED_EDGE ( 'NONE', *, *, #6105, .F. ) ;
#11301 = CARTESIAN_POINT ( 'NONE',  ( 43.01140435219951286, 158.6297705074273381, 29.55568802177586463 ) ) ;
#11302 = LINE ( 'NONE', #9341, #7729 ) ;
#11303 = CARTESIAN_POINT ( 'NONE',  ( 38.01140435219951996, 114.5604996726487457, 32.58608133808903773 ) ) ;
#11304 = CARTESIAN_POINT ( 'NONE',  ( 43.01140435219951286, 69.86518717409400381, 38.86567161673127657 ) ) ;
#11305 = FACE_BOUND ( 'NONE', #11791, .T. ) ;
#11306 = CARTESIAN_POINT ( 'NONE',  ( -157.2955611005345986, -166.4438272943107222, 57.67623309621197336 ) ) ;
#11307 = CARTESIAN_POINT ( 'NONE',  ( -145.2889157411863437, -165.5391397928654555, 41.15050349809589392 ) ) ;
#11308 = CARTESIAN_POINT ( 'NONE',  ( -141.4692556286852891, -180.0630981290892976, 49.65701158161630957 ) ) ;
#11309 =( NAMED_UNIT ( * ) PLANE_ANGLE_UNIT ( ) SI_UNIT ( $, .RADIAN. ) );
#11310 = CARTESIAN_POINT ( 'NONE',  ( 159.4819454078502190, 211.3876867681337046, 4.000000000000021316 ) ) ;
#11311 = CARTESIAN_POINT ( 'NONE',  ( 38.01140435219951996, 155.9344580088726104, 35.83527830041810347 ) ) ;
#11312 = CARTESIAN_POINT ( 'NONE',  ( 47.43856463449118621, 136.8797705074273381, 34.21067981925357060 ) ) ;
#11313 =( BOUNDED_CURVE ( )  B_SPLINE_CURVE ( 2, ( #12724, #1483, #21437, #4340, #21549, #6440, #11390, #1368, #7995, #8100, #16564, #11066, #17780 ),
 .UNSPECIFIED., .F., .F. ) 
 B_SPLINE_CURVE_WITH_KNOTS ( ( 3, 2, 2, 2, 2, 2, 3 ),
 ( 0.7279411764705882026, 0.7294117647058823151, 0.7323529411764705399, 0.7352941176470588758, 0.7382352941176471006, 0.7411764705882353255, 0.7426470588235294379 ),
 .UNSPECIFIED. ) 
 CURVE ( )  GEOMETRIC_REPRESENTATION_ITEM ( )  RATIONAL_B_SPLINE_CURVE ( ( 0.9755282581475768211, 0.9755282581475768211, 1.000000000000000000, 0.9510565162951535312, 1.000000000000000000, 0.9510565162951535312, 1.000000000000000000, 0.9510565162951535312, 1.000000000000000000, 0.9510565162951535312, 1.000000000000000000, 0.9755282581475768211, 0.9755282581475768211 ) ) 
 REPRESENTATION_ITEM ( '' )  );
#11314 = CARTESIAN_POINT ( 'NONE',  ( 75.94266982333172677, 110.2653427511449422, 11.90618179609112026 ) ) ;
#11315 = CARTESIAN_POINT ( 'NONE',  ( 40.27526882409969744, 125.6651871740939868, 30.44471234641812174 ) ) ;
#11316 = CARTESIAN_POINT ( 'NONE',  ( 43.01140435219951996, 10.71049967264875491, 29.21067981925357060 ) ) ;
#11317 = CARTESIAN_POINT ( 'NONE',  ( -142.0420953463936087, -156.6584106276440593, 49.65701158161630957 ) ) ;
#11319 = CARTESIAN_POINT ( 'NONE',  ( 44.55648932407425633, 140.8104996726487457, 29.45539723777780239 ) ) ;
#11318 = AXIS2_PLACEMENT_3D ( 'NONE', #7013, #17231, #15386 ) ;
#11320 = CARTESIAN_POINT ( 'NONE',  ( 23.10700517764660589, 139.6571016847272233, -10.96257334342637435 ) ) ;
#11321 = CARTESIAN_POINT ( 'NONE',  ( -141.4692556286852891, -187.1391397928654499, 52.90620854394536821 ) ) ;
#11322 = VECTOR ( 'NONE', #2259, 1000.000000000000000 ) ;
#11323 = ORIENTED_EDGE ( 'NONE', *, *, #21370, .F. ) ;
#11324 = CARTESIAN_POINT ( 'NONE',  ( -148.3790856849358306, -157.5891397928654953, 59.16757674456786020 ) ) ;
#11325 = ORIENTED_EDGE ( 'NONE', *, *, #5076, .T. ) ;
#11326 = CARTESIAN_POINT ( 'NONE',  ( 48.01140435219951996, 79.28445800887259054, 34.21067981925357060 ) ) ;
#11327 = DIRECTION ( 'NONE',  ( 0.9385982292947088190, 0.3450121214752275289, 0.000000000000000000 ) ) ;
#11328 = PRODUCT_DEFINITION_SHAPE ( 'NONE', 'NONE',  #15648 ) ;
#11329 = CIRCLE ( 'NONE', #20853, 10.00000000000000888 ) ;
#11330 = CARTESIAN_POINT ( 'NONE',  ( 43.01140435219951286, 142.4604996726486945, 39.46799094044489209 ) ) ;
#11332 = CARTESIAN_POINT ( 'NONE',  ( 15.97902590142590462, 112.1642626292039324, 2.851329040111875823 ) ) ;
#11331 = CARTESIAN_POINT ( 'NONE',  ( 41.64333658814960870, 101.5151871740939953, 30.00020018409699318 ) ) ;
#11333 = EDGE_CURVE ( 'NONE', #1303, #16231, #16626, .T. ) ;
#11334 = CARTESIAN_POINT ( 'NONE',  ( -143.8425227516148084, -165.3584106276440480, 44.11586579668791330 ) ) ;
#11335 = CARTESIAN_POINT ( 'NONE',  ( 41.46631938032478359, 60.11049967264874283, 29.45539723777780239 ) ) ;
#11337 = DIRECTION ( 'NONE',  ( 1.000000000000000000, 0.000000000000000000, 0.000000000000000000 ) ) ;
#11336 = CARTESIAN_POINT ( 'NONE',  ( -161.4692556286852891, -178.7130981290893033, 46.40781461928724383 ) ) ;
#11338 = VECTOR ( 'NONE', #13594, 1000.000000000000000 ) ;
#11339 = CARTESIAN_POINT ( 'NONE',  ( 47.05648932407426344, 78.98445800887257917, 37.14960608071593384 ) ) ;
#11340 = CARTESIAN_POINT ( 'NONE',  ( 38.01140435219952707, 78.86049967264872862, 35.83527830041809636 ) ) ;
#11341 = CARTESIAN_POINT ( 'NONE',  ( 47.43856463449117200, 61.46518717409399102, 35.64915139335016647 ) ) ;
#11342 = CARTESIAN_POINT ( 'NONE',  ( 37.24990543953586553, 153.6521207556136517, 3.648881909465930828 ) ) ;
#11343 = CARTESIAN_POINT ( 'NONE',  ( 38.58424406990785371, 153.2651871740940237, 35.64915139335015937 ) ) ;
#11344 = CARTESIAN_POINT ( 'NONE',  ( -142.0420953463935803, -174.2438272943107052, 46.59394152635518793 ) ) ;
#11345 = CARTESIAN_POINT ( 'NONE',  ( -142.0420953463936087, -186.6584106276440309, 49.65701158161630957 ) ) ;
#11346 = EDGE_LOOP ( 'NONE', ( #1133, #4742, #12190, #1035 ) ) ;
#11347 = CARTESIAN_POINT ( 'NONE',  ( 44.37947211624943833, 73.01518717409399528, 38.42115945441014446 ) ) ;
#11348 = CARTESIAN_POINT ( 'NONE',  ( -160.8964159109769696, -167.3084106276440366, 46.59394152635518793 ) ) ;
#11349 = CARTESIAN_POINT ( 'NONE',  ( 55.77169822954404310, 151.7599422098969910, 17.26344356872107255 ) ) ;
#11350 = CARTESIAN_POINT ( 'NONE',  ( -176.9699209214867892, -37.13255853780189852, -19.99999999999995737 ) ) ;
#11351 = CARTESIAN_POINT ( 'NONE',  ( 39.42975644700377558, 135.4151871740940010, 36.81289934271958941 ) ) ;
#11352 = EDGE_CURVE ( 'NONE', #10077, #21815, #21495, .T. ) ;
#11353 = CARTESIAN_POINT ( 'NONE',  ( 18.41688673663920284, 143.6040338654656523, -3.061295755333778512 ) ) ;
#11354 = ORIENTED_EDGE ( 'NONE', *, *, #5830, .T. ) ;
#11355 = ORIENTED_EDGE ( 'NONE', *, *, #3754, .F. ) ;
#11356 = EDGE_CURVE ( 'NONE', #18451, #1608, #18402, .T. ) ;
#11357 = CARTESIAN_POINT ( 'NONE',  ( 71.20918238807936973, 120.1790618917378879, 12.65642078274776416 ) ) ;
#11358 = VERTEX_POINT ( 'NONE', #19953 ) ;
#11359 = ADVANCED_FACE ( 'NONE', ( #4724, #13023 ), #10029, .T. ) ;
#11360 = CARTESIAN_POINT ( 'NONE',  ( 48.01140435219951996, 109.2844580088725905, 34.21067981925357060 ) ) ;
#11361 = CARTESIAN_POINT ( 'NONE',  ( -151.4692556286853176, -164.3130981290893260, 39.65701158161629536 ) ) ;
#11362 = CARTESIAN_POINT ( 'NONE',  ( 38.58424406990784661, 69.22977050742731819, 32.77220824515698183 ) ) ;
#11364 = CARTESIAN_POINT ( 'NONE',  ( 38.24087231542673493, 147.7000375650850970, 3.727681574521009900 ) ) ;
#11363 = CARTESIAN_POINT ( 'NONE',  ( 46.59305225739526435, 124.3151871740940067, 36.81289934271958941 ) ) ;
#11365 = EDGE_CURVE ( 'NONE', #13557, #14220, #4839, .T. ) ;
#11366 = CARTESIAN_POINT ( 'NONE',  ( 44.55648932407425633, 92.81049967264874567, 29.45539723777780239 ) ) ;
#11367 = CARTESIAN_POINT ( 'NONE',  ( 134.6380592378699532, 268.5785371414991687, -19.99999999999997868 ) ) ;
#11368 = CARTESIAN_POINT ( 'NONE',  ( 39.03656800816600736, 95.22440407761430947, 31.15999777443385454 ) ) ;
#11369 = FACE_OUTER_BOUND ( 'NONE', #6880, .T. ) ;
#11370 = CARTESIAN_POINT ( 'NONE',  ( 47.43856463449117200, 88.46518717409399812, 35.64915139335016647 ) ) ;
#11371 = CARTESIAN_POINT ( 'NONE',  ( 137.5268905834513191, 193.0332408774651185, -44.99999999999997158 ) ) ;
#11372 = CYLINDRICAL_SURFACE ( 'NONE', #3939, 10.00000000000000888 ) ;
#11373 = ORIENTED_EDGE ( 'NONE', *, *, #4463, .T. ) ;
#11374 = CARTESIAN_POINT ( 'NONE',  ( 38.58424406990784661, 75.52977050742732956, 35.64915139335016647 ) ) ;
#11375 = CARTESIAN_POINT ( 'NONE',  ( -154.3824083646099439, -191.7584106276440536, 40.69124936498395328 ) ) ;
#11376 = CARTESIAN_POINT ( 'NONE',  ( 12.03843011909301453, 134.4860913190374561, 2.577281550626734141 ) ) ;
#11377 = CARTESIAN_POINT ( 'NONE',  ( -157.2955611005346270, -181.7084106276440423, 57.67623309621198047 ) ) ;
#11378 = ORIENTED_EDGE ( 'NONE', *, *, #18933, .T. ) ;
#11379 = CARTESIAN_POINT ( 'NONE',  ( -161.4692556286853176, -161.4891397928654726, 49.65701158161630957 ) ) ;
#11380 = CARTESIAN_POINT ( 'NONE',  ( 5.130598475945862827E-15, 0.000000000000000000, 10.00000000000001599 ) ) ;
#11381 =( BOUNDED_CURVE ( )  B_SPLINE_CURVE ( 2, ( #6429, #18446, #5001, #13373, #14903, #6318, #18556, #8202, #6666, #13044, #15132, #20110, #13151 ),
 .UNSPECIFIED., .F., .F. ) 
 B_SPLINE_CURVE_WITH_KNOTS ( ( 3, 2, 2, 2, 2, 2, 3 ),
 ( 0.8392857142857143016, 0.8428571428571428603, 0.8499999999999999778, 0.8571428571428570953, 0.8642857142857143238, 0.8714285714285714413, 0.8750000000000000000 ),
 .UNSPECIFIED. ) 
 CURVE ( )  GEOMETRIC_REPRESENTATION_ITEM ( )  RATIONAL_B_SPLINE_CURVE ( ( 0.9755282581475768211, 0.9755282581475768211, 1.000000000000000000, 0.9510565162951535312, 1.000000000000000000, 0.9510565162951535312, 1.000000000000000000, 0.9510565162951535312, 1.000000000000000000, 0.9510565162951535312, 1.000000000000000000, 0.9755282581475768211, 0.9755282581475768211 ) ) 
 REPRESENTATION_ITEM ( '' )  );
#11382 = CARTESIAN_POINT ( 'NONE',  ( 39.42975644700377558, 126.0797705074273267, 31.60846029578754468 ) ) ;
#11383 = ORIENTED_EDGE ( 'NONE', *, *, #14444, .F. ) ;
#11384 = EDGE_CURVE ( 'NONE', #21749, #20722, #6382, .T. ) ;
#11385 = DIRECTION ( 'NONE',  ( 0.000000000000000000, 0.000000000000000000, -1.000000000000000000 ) ) ;
#11386 = VERTEX_POINT ( 'NONE', #6617 ) ;
#11387 = LINE ( 'NONE', #19546, #17461 ) ;
#11388 = CARTESIAN_POINT ( 'NONE',  ( 46.59305225739526435, 154.9151871740940010, 31.60846029578754468 ) ) ;
#11389 = CARTESIAN_POINT ( 'NONE',  ( 147.5268905834513475, 193.0332408774651185, -19.99999999999997868 ) ) ;
#11390 = CARTESIAN_POINT ( 'NONE',  ( 38.01140435219952707, 83.78445800887257633, 34.21067981925357060 ) ) ;
#11391 = CARTESIAN_POINT ( 'NONE',  ( -143.3790856849358306, -187.2891397928654555, 55.53486410454105027 ) ) ;
#11392 = CARTESIAN_POINT ( 'NONE',  ( 41.46631938032478359, 89.18445800887258201, 29.45539723777780239 ) ) ;
#11393 = CYLINDRICAL_SURFACE ( 'NONE', #8662, 10.00000000000000888 ) ;
#11394 = CARTESIAN_POINT ( 'NONE',  ( -160.8964159109769696, -190.8938272943107393, 49.65701158161630957 ) ) ;
#11395 = CARTESIAN_POINT ( 'NONE',  ( 39.92123440845004723, 119.3344580088725735, 29.95742577749337343 ) ) ;
#11396 = CARTESIAN_POINT ( 'NONE',  ( 45.74753988029933538, 106.4297705074273068, 37.97664729208901946 ) ) ;
#11397 = CARTESIAN_POINT ( 'NONE',  ( 17.64326796073342862, 132.3496329740814303, 22.67862939001841127 ) ) ;
#11398 = CARTESIAN_POINT ( 'NONE',  ( -148.5561028927606344, -179.7938272943107449, 40.69124936498395328 ) ) ;
#11399 = VECTOR ( 'NONE', #530, 1000.000000000000000 ) ;
#11400 = CARTESIAN_POINT ( 'NONE',  ( 47.43856463449118621, 91.61518717409400381, 34.21067981925357060 ) ) ;
#11401 = CARTESIAN_POINT ( 'NONE',  ( 147.8787791192428074, -126.9891397928655010, 39.65701158161628825 ) ) ;
#11402 = ORIENTED_EDGE ( 'NONE', *, *, #4063, .T. ) ;
#11403 = CARTESIAN_POINT ( 'NONE',  ( -19.70755683829218796, -31.26594044116892590, 4.000000000000021316 ) ) ;
#11404 = CARTESIAN_POINT ( 'NONE',  ( 62.84376099716368458, 92.00366499689042143, 13.64888190966157566 ) ) ;
#11405 = CARTESIAN_POINT ( 'NONE',  ( 16.30727314429931241, 128.7156746967485788, -10.48204345529337189 ) ) ;
#11406 = CARTESIAN_POINT ( 'NONE',  ( 44.37947211624943833, 64.27977050742731535, 38.42115945441014446 ) ) ;
#11407 = ORIENTED_EDGE ( 'NONE', *, *, #17355, .F. ) ;
#11408 = VERTEX_POINT ( 'NONE', #13333 ) ;
#11409 = CARTESIAN_POINT ( 'NONE',  ( 45.74753988029933538, 148.4297705074273210, 37.97664729208901946 ) ) ;
#11410 = DIRECTION ( 'NONE',  ( 1.000000000000000000, 0.000000000000000000, -1.140132994654635861E-16 ) ) ;
#11411 = AXIS2_PLACEMENT_3D ( 'NONE', #12976, #4701, #4591 ) ;
#11412 = CARTESIAN_POINT ( 'NONE',  ( 38.01140435219952707, 108.7104996726487514, 34.21067981925357060 ) ) ;
#11413 = CARTESIAN_POINT ( 'NONE',  ( 43.01140435219951286, 63.86518717409398960, 38.86567161673127657 ) ) ;
#11414 = DIRECTION ( 'NONE',  ( 0.000000000000000000, 1.000000000000000000, 0.000000000000000000 ) ) ;
#11415 = PRESENTATION_LAYER_ASSIGNMENT (  '', '', ( #8969 ) ) ;
#11416 = CARTESIAN_POINT ( 'NONE',  ( -143.8425227516148084, -159.6938272943107222, 55.19815736654470584 ) ) ;
#11417 = CARTESIAN_POINT ( 'NONE',  ( 41.46631938032478359, 156.3844580088725706, 38.96596240072933170 ) ) ;
#11418 = CARTESIAN_POINT ( 'NONE',  ( -157.6495955161842062, -175.1130981290892521, 58.16351966513671812 ) ) ;
#11419 = CARTESIAN_POINT ( 'NONE',  ( 0.000000000000000000, 0.000000000000000000, 0.000000000000000000 ) ) ;
#11420 = LINE ( 'NONE', #6360, #14938 ) ;
#11421 = CARTESIAN_POINT ( 'NONE',  ( 45.74753988029933538, 128.3297705074273267, 30.44471234641811819 ) ) ;
#11422 = CARTESIAN_POINT ( 'NONE',  ( 18.00183652574411397, 143.4013020786237860, 8.929911949387623338 ) ) ;
#11423 = CARTESIAN_POINT ( 'NONE',  ( 40.27526882409969744, 117.5651871740940067, 37.97664729208901235 ) ) ;
#11424 = EDGE_CURVE ( 'NONE', #4573, #4975, #14503, .T. ) ;
#11425 = CARTESIAN_POINT ( 'NONE',  ( -161.4692556286853176, -182.4891397928654726, 49.65701158161630957 ) ) ;
#11426 = CARTESIAN_POINT ( 'NONE',  ( 39.92123440845005433, 151.1604996726487116, 38.46393386101375711 ) ) ;
#11427 = CARTESIAN_POINT ( 'NONE',  ( 45.51141300902961717, 59.09387774407727534, 29.88055779818149915 ) ) ;
#11428 = CARTESIAN_POINT ( 'NONE',  ( -47.86331837773882825, 0.000000000000000000, -25.00000000000000000 ) ) ;
#11429 = CARTESIAN_POINT ( 'NONE',  ( 19.58029209685692962, 104.0714924419353480, 21.50917333468608561 ) ) ;
#11430 = CARTESIAN_POINT ( 'NONE',  ( -149.8854112254399524, -186.3160212151857422, 39.65701158161630246 ) ) ;
#11431 = CARTESIAN_POINT ( 'NONE',  ( 46.59305225739526435, 91.57977050742731251, 36.81289934271958941 ) ) ;
#11432 = EDGE_LOOP ( 'NONE', ( #5210, #1066, #11821, #19823 ) ) ;
#11433 = VECTOR ( 'NONE', #21009, 1000.000000000000000 ) ;
#11434 = CARTESIAN_POINT ( 'NONE',  ( 43.01140435219951996, 10.71049967264875491, 34.21067981925357060 ) ) ;
#11435 = EDGE_LOOP ( 'NONE', ( #18821, #11689, #9877, #5324, #10643, #13042 ) ) ;
#11436 = CARTESIAN_POINT ( 'NONE',  ( 38.96631938032478359, 78.08445800887257349, 37.14960608071593384 ) ) ;
#11437 = CARTESIAN_POINT ( 'NONE',  ( 43.01140435219951286, 59.96049967264874425, 29.21067981925356705 ) ) ;
#11438 = CARTESIAN_POINT ( 'NONE',  ( 47.05648932407426344, 137.5104996726487627, 31.27175355779120025 ) ) ;
#11440 = CARTESIAN_POINT ( 'NONE',  ( 30.56769828357572294, 94.69056354510921381, 8.922930725513751327 ) ) ;
#11439 = CARTESIAN_POINT ( 'NONE',  ( 38.58424406990784661, 93.26518717409399528, 35.64915139335016647 ) ) ;
#11441 =( BOUNDED_CURVE ( )  B_SPLINE_CURVE ( 2, ( #13570, #8299, #16770, #23, #3223, #9955, #16659, #8412, #135, #1571, #10175, #18545, #16875 ),
 .UNSPECIFIED., .F., .F. ) 
 B_SPLINE_CURVE_WITH_KNOTS ( ( 3, 2, 2, 2, 2, 2, 3 ),
 ( 0.7573529411764705621, 0.7588235294117646745, 0.7617647058823528994, 0.7647058823529411242, 0.7676470588235294601, 0.7705882352941176849, 0.7720588235294117974 ),
 .UNSPECIFIED. ) 
 CURVE ( )  GEOMETRIC_REPRESENTATION_ITEM ( )  RATIONAL_B_SPLINE_CURVE ( ( 0.9755282581475768211, 0.9755282581475768211, 1.000000000000000000, 0.9510565162951535312, 1.000000000000000000, 0.9510565162951535312, 1.000000000000000000, 0.9510565162951535312, 1.000000000000000000, 0.9510565162951535312, 1.000000000000000000, 0.9755282581475768211, 0.9755282581475768211 ) ) 
 REPRESENTATION_ITEM ( '' )  );
#11442 = CARTESIAN_POINT ( 'NONE',  ( -142.0420953463936087, -168.6584106276440593, 49.65701158161630957 ) ) ;
#11443 = CARTESIAN_POINT ( 'NONE',  ( -159.0959885057557983, -190.5938272943107279, 55.19815736654470584 ) ) ;
#11445 = FACE_OUTER_BOUND ( 'NONE', #7473, .T. ) ;
#11444 = DIRECTION ( 'NONE',  ( 0.000000000000000000, 0.000000000000000000, 1.000000000000000000 ) ) ;
#11446 = LINE ( 'NONE', #9815, #5598 ) ;
#11447 = CARTESIAN_POINT ( 'NONE',  ( -145.2889157411863437, -177.5130981290893430, 58.16351966513671812 ) ) ;
#11448 = CARTESIAN_POINT ( 'NONE',  ( 47.05648932407426344, 114.9844580088725792, 37.14960608071593384 ) ) ;
#11449 = CARTESIAN_POINT ( 'NONE',  ( 45.74753988029933538, 61.16518717409398675, 37.97664729208901946 ) ) ;
#11450 = CARTESIAN_POINT ( 'NONE',  ( -47.86331837773882825, -19.06233958201669765, -35.00000000000000000 ) ) ;
#11451 = CARTESIAN_POINT ( 'NONE',  ( 76.79083979644461522, 114.3551126354810492, -1.232281421064668869 ) ) ;
#11452 = CARTESIAN_POINT ( 'NONE',  ( -159.0959885057557983, -158.1938272943107222, 44.11586579668791330 ) ) ;
#11453 = CARTESIAN_POINT ( 'NONE',  ( -160.8964159109769696, -188.1584106276440593, 49.65701158161630957 ) ) ;
#11454 = ORIENTED_EDGE ( 'NONE', *, *, #12450, .F. ) ;
#11455 = CARTESIAN_POINT ( 'NONE',  ( 47.43856463449117911, 70.46518717409401233, 35.64915139335015937 ) ) ;
#11456 = CARTESIAN_POINT ( 'NONE',  ( -154.3824083646099439, -172.5584106276440366, 58.62277379824867296 ) ) ;
#11457 = CARTESIAN_POINT ( 'NONE',  ( 28.23826046203858908, 88.93502212982269839, 20.83457506318435648 ) ) ;
#11458 = DIRECTION ( 'NONE',  ( 0.000000000000000000, 0.000000000000000000, 1.000000000000000000 ) ) ;
#11459 = CARTESIAN_POINT ( 'NONE',  ( 38.58424406990784661, 126.2651871740940237, 35.64915139335016647 ) ) ;
#11460 = ADVANCED_FACE ( 'NONE', ( #16041 ), #18543, .T. ) ;
#11461 = CARTESIAN_POINT ( 'NONE',  ( 71.58903643207423784, 138.6103067756119742, -8.061014907923841122 ) ) ;
#11462 = ORIENTED_EDGE ( 'NONE', *, *, #12200, .F. ) ;
#11463 = ORIENTED_EDGE ( 'NONE', *, *, #14609, .F. ) ;
#11464 = CARTESIAN_POINT ( 'NONE',  ( 65.44800906011916197, 136.9904114405718758, 11.94221925691594777 ) ) ;
#11465 = VERTEX_POINT ( 'NONE', #2748 ) ;
#11466 = DIRECTION ( 'NONE',  ( -0.000000000000000000, 0.000000000000000000, -1.000000000000000000 ) ) ;
#11467 = AXIS2_PLACEMENT_3D ( 'NONE', #15201, #15523, #7048 ) ;
#11468 = CARTESIAN_POINT ( 'NONE',  ( 45.74753988029933538, 65.32977050742732672, 30.44471234641811819 ) ) ;
#11470 = CARTESIAN_POINT ( 'NONE',  ( 18.57470074671828542, 105.8336742703428257, 1.585105279193314010 ) ) ;
#11469 = CARTESIAN_POINT ( 'NONE',  ( 47.43856463449118621, 124.6151871740940038, 34.21067981925357060 ) ) ;
#11471 = CARTESIAN_POINT ( 'NONE',  ( 39.92123440845004723, 82.16049967264871157, 38.46393386101376421 ) ) ;
#11472 = DIRECTION ( 'NONE',  ( 0.4999999999999993894, 0.000000000000000000, -0.8660254037844389297 ) ) ;
#11473 = EDGE_CURVE ( 'NONE', #7305, #13261, #12563, .T. ) ;
#11474 = DIRECTION ( 'NONE',  ( 0.000000000000000000, 0.000000000000000000, 1.000000000000000000 ) ) ;
#11475 = EDGE_CURVE ( 'NONE', #9722, #1696, #879, .T. ) ;
#11476 = CARTESIAN_POINT ( 'NONE',  ( 46.59305225739526435, 85.91518717409400097, 31.60846029578754468 ) ) ;
#11477 = CARTESIAN_POINT ( 'NONE',  ( 43.01140435219951996, 150.5344580088725763, 39.21067981925356349 ) ) ;
#11478 = CARTESIAN_POINT ( 'NONE',  ( -161.4692556286852891, -185.3391397928654953, 52.90620854394536821 ) ) ;
#11479 = VERTEX_POINT ( 'NONE', #16186 ) ;
#11480 = CARTESIAN_POINT ( 'NONE',  ( 40.27526882409969033, 62.92977050742729972, 30.44471234641811819 ) ) ;
#11481 = CARTESIAN_POINT ( 'NONE',  ( -148.5561028927606344, -155.7938272943107449, 40.69124936498395328 ) ) ;
#11482 = EDGE_CURVE ( 'NONE', #8663, #9959, #19968, .T. ) ;
#11483 = CIRCLE ( 'NONE', #3758, 10.00000000000000888 ) ;
#11484 = CARTESIAN_POINT ( 'NONE',  ( 45.29500579500201951, 154.0643053174194961, 10.91066218119221709 ) ) ;
#11485 = CARTESIAN_POINT ( 'NONE',  ( -160.8964159109769696, -188.0084106276440252, 52.72008163687743121 ) ) ;
#11486 = CIRCLE ( 'NONE', #15376, 10.00000000000000888 ) ;
#11487 = ORIENTED_EDGE ( 'NONE', *, *, #12907, .F. ) ;
#11488 = CARTESIAN_POINT ( 'NONE',  ( 126.8576204525573274, -126.9891397928655010, -17.64809332337413750 ) ) ;
#11489 = CIRCLE ( 'NONE', #3043, 10.00000000000000888 ) ;
#11490 = CARTESIAN_POINT ( 'NONE',  ( 43.01140435219951996, 10.71049967264875491, 39.21067981925356349 ) ) ;
#11491 = CARTESIAN_POINT ( 'NONE',  ( 47.43856463449118621, 124.8797705074273239, 34.21067981925357060 ) ) ;
#11492 = CARTESIAN_POINT ( 'NONE',  ( 39.42188022582085694, 153.9507182763122159, -10.27990332573616961 ) ) ;
#11493 = ORIENTED_EDGE ( 'NONE', *, *, #693, .F. ) ;
#11494 = DIRECTION ( 'NONE',  ( 0.000000000000000000, 0.000000000000000000, 1.000000000000000000 ) ) ;
#11495 = ORIENTED_EDGE ( 'NONE', *, *, #72, .T. ) ;
#11496 = CARTESIAN_POINT ( 'NONE',  ( 39.42975644700377558, 117.0797705074273267, 31.60846029578754468 ) ) ;
#11497 = DIRECTION ( 'NONE',  ( 0.3450121214752278065, -0.9385982292947087080, -0.000000000000000000 ) ) ;
#11498 = CARTESIAN_POINT ( 'NONE',  ( 41.64333658814960870, 86.77977050742731535, 30.00020018409699318 ) ) ;
#11499 = CARTESIAN_POINT ( 'NONE',  ( 45.74753988029933538, 154.1651871740939441, 37.97664729208901946 ) ) ;
#11500 = VECTOR ( 'NONE', #2749, 1000.000000000000000 ) ;
#11501 = DIRECTION ( 'NONE',  ( -1.000000000000000000, 0.000000000000000000, 0.000000000000000000 ) ) ;
#11502 = CARTESIAN_POINT ( 'NONE',  ( 41.46631938032478359, 102.3844580088725849, 38.96596240072933170 ) ) ;
#11503 = CARTESIAN_POINT ( 'NONE',  ( -151.4692556286852891, -126.9891397928655010, -54.65701158161630246 ) ) ;
#11504 = CARTESIAN_POINT ( 'NONE',  ( -141.4692556286852891, -181.1391397928654783, 52.90620854394536821 ) ) ;
#11505 = DIRECTION ( 'NONE',  ( 0.000000000000000000, 1.000000000000000000, 0.000000000000000000 ) ) ;
#11506 = CARTESIAN_POINT ( 'NONE',  ( 48.01140435219951996, 131.3604996726487002, 32.58608133808903773 ) ) ;
#11507 = CARTESIAN_POINT ( 'NONE',  ( -143.8425227516148084, -192.6938272943107222, 55.19815736654470584 ) ) ;
#11508 = ITEM_DEFINED_TRANSFORMATION ( 'NONE', 'NONE', #14424,  #12657 ) ;
#11509 = CARTESIAN_POINT ( 'NONE',  ( 38.01140435219951996, 122.6344580088725849, 32.58608133808903773 ) ) ;
#11510 = CARTESIAN_POINT ( 'NONE',  ( 40.27526882409969033, 105.8297705074273125, 37.97664729208901946 ) ) ;
#11511 =( BOUNDED_CURVE ( )  B_SPLINE_CURVE ( 2, ( #19872, #11157, #6309, #3224, #19991, #4876, #7866, #11478, #3114, #9845, #6421, #16118, #19531 ),
 .UNSPECIFIED., .F., .F. ) 
 B_SPLINE_CURVE_WITH_KNOTS ( ( 3, 2, 2, 2, 2, 2, 3 ),
 ( 0.2321428571428571508, 0.2357142857142857095, 0.2428571428571428548, 0.2500000000000000000, 0.2571428571428571175, 0.2642857142857142905, 0.2678571428571429047 ),
 .UNSPECIFIED. ) 
 CURVE ( )  GEOMETRIC_REPRESENTATION_ITEM ( )  RATIONAL_B_SPLINE_CURVE ( ( 0.9755282581475767101, 0.9755282581475768211, 1.000000000000000000, 0.9510565162951535312, 1.000000000000000000, 0.9510565162951535312, 1.000000000000000000, 0.9510565162951535312, 1.000000000000000000, 0.9510565162951535312, 1.000000000000000000, 0.9755282581475763770, 0.9755282581475768211 ) ) 
 REPRESENTATION_ITEM ( '' )  );
#11512 = CARTESIAN_POINT ( 'NONE',  ( 26.22827968769296092, 97.14409021710402214, 14.12817222279094942 ) ) ;
#11513 = CARTESIAN_POINT ( 'NONE',  ( -145.6429501568359797, -186.8438272943106995, 57.67623309621198047 ) ) ;
#11514 = CARTESIAN_POINT ( 'NONE',  ( 44.37947211624943833, 85.01518717409399528, 38.42115945441014446 ) ) ;
#11515 = CARTESIAN_POINT ( 'NONE',  ( 43.01140435219951996, 144.9070776186055696, 29.21067981925357060 ) ) ;
#11516 = EDGE_LOOP ( 'NONE', ( #4042, #4385, #9616, #13366 ) ) ;
#11517 = CARTESIAN_POINT ( 'NONE',  ( 173.3794444120442222, -354.7018910364275257, 19.99999999999999645 ) ) ;
#11518 = CARTESIAN_POINT ( 'NONE',  ( -260.7034334617478066, 709.2382145066653720, 0.000000000000000000 ) ) ;
#11519 = VECTOR ( 'NONE', #9322, 1000.000000000000000 ) ;
#11520 = CARTESIAN_POINT ( 'NONE',  ( 32.71008791447857789, 146.0719641954536883, -2.505641559509553140 ) ) ;
#11521 = PRODUCT_DEFINITION_SHAPE ( 'NONE', 'NONE',  #21823 ) ;
#11522 = CARTESIAN_POINT ( 'NONE',  ( 43.01140435219951286, 70.12977050742730967, 38.86567161673127657 ) ) ;
#11523 = ORIENTED_EDGE ( 'NONE', *, *, #20597, .T. ) ;
#11524 = CARTESIAN_POINT ( 'NONE',  ( 46.59305225739526435, 148.5797705074273267, 36.81289934271958941 ) ) ;
#11525 = CARTESIAN_POINT ( 'NONE',  ( 44.37947211624943833, 98.47977050742731819, 30.00020018409699318 ) ) ;
#11526 = CARTESIAN_POINT ( 'NONE',  ( 41.46631938032478359, 141.1104996726487286, 29.45539723777780239 ) ) ;
#11527 = AXIS2_PLACEMENT_3D ( 'NONE', #9663, #18127, #19795 ) ;
#11528 = EDGE_CURVE ( 'NONE', #10070, #9693, #15398, .T. ) ;
#11529 = CARTESIAN_POINT ( 'NONE',  ( 43.01140435219951286, 106.4604996726487371, 39.46799094044489209 ) ) ;
#11530 = CARTESIAN_POINT ( 'NONE',  ( 38.58424406990784661, 65.96518717409399812, 32.77220824515698183 ) ) ;
#11531 = CARTESIAN_POINT ( 'NONE',  ( 39.92123440845005433, 95.33445800887255928, 29.95742577749336988 ) ) ;
#11532 = CARTESIAN_POINT ( 'NONE',  ( -154.3824083646099439, -160.2938272943107449, 58.62277379824867296 ) ) ;
#11533 = VECTOR ( 'NONE', #17115, 1000.000000000000000 ) ;
#11534 = CARTESIAN_POINT ( 'NONE',  ( 163.3401611601853460, 191.7221236944927796, 21.49552782297503128 ) ) ;
#11535 = CARTESIAN_POINT ( 'NONE',  ( -148.3790856849358306, -177.6630981290893203, 59.16757674456786020 ) ) ;
#11536 =( NAMED_UNIT ( * ) SI_UNIT ( $, .STERADIAN. ) SOLID_ANGLE_UNIT ( ) );
#11537 = CARTESIAN_POINT ( 'NONE',  ( -153.0531000319306258, -192.1622583705451746, 39.65701158161628115 ) ) ;
#11538 = CARTESIAN_POINT ( 'NONE',  ( 41.64333658814960870, 134.7797705074273154, 30.00020018409699318 ) ) ;
#11539 = CARTESIAN_POINT ( 'NONE',  ( 76.43728072391715500, 127.6653364257898744, 18.33484128816649772 ) ) ;
#11540 = CARTESIAN_POINT ( 'NONE',  ( 40.27526882409969744, 116.6651871740939868, 30.44471234641812174 ) ) ;
#11541 = CARTESIAN_POINT ( 'NONE',  ( -153.0531000319306827, -181.8160212151857422, 59.65701158161632378 ) ) ;
#11542 = CARTESIAN_POINT ( 'NONE',  ( -151.4692556286852607, -168.2391397928654442, 39.65701158161629536 ) ) ;
#11543 = APPLICATION_CONTEXT ( 'automotive_design' ) ;
#11544 = CARTESIAN_POINT ( 'NONE',  ( 43.80332655382220963, 140.8836182503284817, 29.21067981925357060 ) ) ;
#11545 = CARTESIAN_POINT ( 'NONE',  ( 72.37431012622080573, 137.3510900982057308, 5.986230922049878167 ) ) ;
#11546 = CARTESIAN_POINT ( 'NONE',  ( 29.22050282933603071, 144.5044581412665536, -3.652897588741476742 ) ) ;
#11547 = CYLINDRICAL_SURFACE ( 'NONE', #2299, 10.00000000000000888 ) ;
#11548 = CARTESIAN_POINT ( 'NONE',  ( 38.58424406990785371, 99.22977050742731819, 32.77220824515697473 ) ) ;
#11549 = ORIENTED_EDGE ( 'NONE', *, *, #2767, .F. ) ;
#11550 = FACE_OUTER_BOUND ( 'NONE', #15777, .T. ) ;
#11551 = ORIENTED_EDGE ( 'NONE', *, *, #16699, .F. ) ;
#11552 = CARTESIAN_POINT ( 'NONE',  ( 46.10157429594899270, 82.73445800887257917, 29.95742577749337343 ) ) ;
#11553 = CARTESIAN_POINT ( 'NONE',  ( 147.8787791192428074, -126.9891397928655010, 49.65701158161629536 ) ) ;
#11554 = EDGE_CURVE ( 'NONE', #17105, #17591, #8696, .T. ) ;
#11555 = CARTESIAN_POINT ( 'NONE',  ( 43.01140435219951286, 137.9604996726487229, 28.95336869806222779 ) ) ;
#11557 = CARTESIAN_POINT ( 'NONE',  ( 14.91610048035210312, 121.0785340954179645, 3.208644154750278865 ) ) ;
#11556 = CARTESIAN_POINT ( 'NONE',  ( 40.27526882409969033, 99.56518717409400665, 37.97664729208901946 ) ) ;
#11558 = CARTESIAN_POINT ( 'NONE',  ( -151.4692556286852891, -163.4084106276440309, 59.56931450028537967 ) ) ;
#11559 = CARTESIAN_POINT ( 'NONE',  ( -148.5561028927606344, -186.9938272943107336, 58.62277379824867296 ) ) ;
#11561 = CARTESIAN_POINT ( 'NONE',  ( 43.01140435219951996, 10.71049967264875491, 34.21067981925357060 ) ) ;
#11560 = CARTESIAN_POINT ( 'NONE',  ( -159.5594255724347761, -178.2630981290893146, 55.53486410454104316 ) ) ;
#11562 = CARTESIAN_POINT ( 'NONE',  ( -143.3790856849358306, -188.7630981290893146, 43.77915905869157598 ) ) ;
#11563 = CARTESIAN_POINT ( 'NONE',  ( 41.46631938032478359, 148.3104996726487457, 38.96596240072933170 ) ) ;
#11564 = CARTESIAN_POINT ( 'NONE',  ( 47.05648932407426344, 115.5844580088725877, 31.27175355779120025 ) ) ;
#11565 = CARTESIAN_POINT ( 'NONE',  ( 47.43856463449118621, 64.61518717409398960, 34.21067981925357060 ) ) ;
#11566 = CARTESIAN_POINT ( 'NONE',  ( -54.92240467314265828, 790.2067769114943303, -0.8325491102011938205 ) ) ;
#11567 = CARTESIAN_POINT ( 'NONE',  ( 76.66991938639012005, 113.6622739410785670, 5.791450954060403333 ) ) ;
#11568 = CARTESIAN_POINT ( 'NONE',  ( 38.58424406990785371, 144.2651871740939953, 35.64915139335015937 ) ) ;
#11569 = CARTESIAN_POINT ( 'NONE',  ( -159.0959885057557983, -163.5938272943107279, 55.19815736654470584 ) ) ;
#11570 = CARTESIAN_POINT ( 'NONE',  ( -142.0420953463936087, -177.6584106276440309, 49.65701158161630957 ) ) ;
#11571 = ORIENTED_EDGE ( 'NONE', *, *, #16281, .F. ) ;
#11572 = CARTESIAN_POINT ( 'NONE',  ( 39.92123440845005433, 77.33445800887257349, 29.95742577749336988 ) ) ;
#11573 = CARTESIAN_POINT ( 'NONE',  ( -151.4692556286852891, -163.4084106276440309, 59.56931450028537967 ) ) ;
#11574 = CARTESIAN_POINT ( 'NONE',  ( 45.08439497331802670, 154.1588294112744677, 16.90626985941621641 ) ) ;
#11575 = DIRECTION ( 'NONE',  ( 1.000000000000000000, 0.000000000000000000, -0.000000000000000000 ) ) ;
#11576 = CARTESIAN_POINT ( 'NONE',  ( 38.58424406990784661, 129.2651871740940237, 35.64915139335016647 ) ) ;
#11577 = CARTESIAN_POINT ( 'NONE',  ( 47.68298272704948459, 153.7393326413893817, -9.013488496775837078 ) ) ;
#11578 = ORIENTED_EDGE ( 'NONE', *, *, #11278, .T. ) ;
#11579 = ORIENTED_EDGE ( 'NONE', *, *, #3982, .F. ) ;
#11580 = DIRECTION ( 'NONE',  ( 0.000000000000000000, 0.000000000000000000, 1.000000000000000000 ) ) ;
#11581 = ORIENTED_EDGE ( 'NONE', *, *, #19885, .F. ) ;
#11582 =( BOUNDED_CURVE ( )  B_SPLINE_CURVE ( 2, ( #10016, #5267, #18713, #13530, #16832, #10342, #17045, #18607, #20265, #10453, #8689, #3511, #13319 ),
 .UNSPECIFIED., .F., .F. ) 
 B_SPLINE_CURVE_WITH_KNOTS ( ( 3, 2, 2, 2, 2, 2, 3 ),
 ( 0.1964285714285714524, 0.2000000000000000111, 0.2071428571428571563, 0.2142857142857142738, 0.2214285714285714191, 0.2285714285714285643, 0.2321428571428571508 ),
 .UNSPECIFIED. ) 
 CURVE ( )  GEOMETRIC_REPRESENTATION_ITEM ( )  RATIONAL_B_SPLINE_CURVE ( ( 0.9755282581475767101, 0.9755282581475768211, 1.000000000000000000, 0.9510565162951535312, 1.000000000000000000, 0.9510565162951535312, 1.000000000000000000, 0.9510565162951535312, 1.000000000000000000, 0.9510565162951535312, 1.000000000000000000, 0.9755282581475765991, 0.9755282581475767101 ) ) 
 REPRESENTATION_ITEM ( '' )  );
#11583 = CARTESIAN_POINT ( 'NONE',  ( 38.01140435219952707, 110.7844580088725905, 34.21067981925357060 ) ) ;
#11584 = CARTESIAN_POINT ( 'NONE',  ( 40.27526882409969744, 153.8297705074273267, 37.97664729208901235 ) ) ;
#11585 = VECTOR ( 'NONE', #12309, 1000.000000000000000 ) ;
#11586 = CARTESIAN_POINT ( 'NONE',  ( 47.43856463449117200, 64.72977050742731819, 35.64915139335016647 ) ) ;
#11588 = CARTESIAN_POINT ( 'NONE',  ( 18.92353847440636727, 134.5693106245527702, 2.775393258647981920 ) ) ;
#11587 = CARTESIAN_POINT ( 'NONE',  ( 47.43856463449117200, 127.7651871740940237, 32.77220824515698183 ) ) ;
#11589 = CARTESIAN_POINT ( 'NONE',  ( 38.96631938032478359, 79.01049967264873430, 37.14960608071593384 ) ) ;
#11590 = CARTESIAN_POINT ( 'NONE',  ( 18.14018356548558941, 143.3940520581896862, 16.92415443696469879 ) ) ;
#11591 = CARTESIAN_POINT ( 'NONE',  ( 46.10157429594899270, 98.66049967264872578, 29.95742577749336988 ) ) ;
#11592 = DIRECTION ( 'NONE',  ( 0.000000000000000000, 0.000000000000000000, 1.000000000000000000 ) ) ;
#11593 = CARTESIAN_POINT ( 'NONE',  ( 41.64333658814960870, 92.51518717409399528, 30.00020018409699318 ) ) ;
#11594 = DIRECTION ( 'NONE',  ( -0.9385982292947088190, -0.3450121214752274179, 2.040824802394967185E-16 ) ) ;
#11595 = CARTESIAN_POINT ( 'NONE',  ( 47.05648932407426344, 141.9844580088725650, 37.14960608071593384 ) ) ;
#11596 = VERTEX_POINT ( 'NONE', #1944 ) ;
#11597 = CARTESIAN_POINT ( 'NONE',  ( 47.43856463449117200, 65.02977050742732956, 32.77220824515698183 ) ) ;
#11598 = CARTESIAN_POINT ( 'NONE',  ( -151.4692556286852891, -157.1438272943107393, 59.56931450028537967 ) ) ;
#11599 = CARTESIAN_POINT ( 'NONE',  ( 76.66991938639012005, 113.6622739410785670, 5.791450954060403333 ) ) ;
#11600 = CARTESIAN_POINT ( 'NONE',  ( -159.0959885057557983, -187.8584106276440480, 55.19815736654470584 ) ) ;
#11601 = ORIENTED_EDGE ( 'NONE', *, *, #13459, .T. ) ;
#11602 = CARTESIAN_POINT ( 'NONE',  ( 41.64333658814960870, 149.5151871740940237, 30.00020018409699318 ) ) ;
#11603 =( GEOMETRIC_REPRESENTATION_CONTEXT ( 3 ) GLOBAL_UNCERTAINTY_ASSIGNED_CONTEXT ( ( #13497 ) ) GLOBAL_UNIT_ASSIGNED_CONTEXT ( ( #857, #4589, #12863 ) ) REPRESENTATION_CONTEXT ( 'NONE', 'WORKASPACE' ) );
#11604 = EDGE_CURVE ( 'NONE', #7553, #4466, #14333, .T. ) ;
#11605 = DIRECTION ( 'NONE',  ( 0.000000000000000000, 0.000000000000000000, 1.000000000000000000 ) ) ;
#11606 = CARTESIAN_POINT ( 'NONE',  ( 41.64333658814960870, 117.9797705074273182, 38.42115945441014446 ) ) ;
#11607 = CARTESIAN_POINT ( 'NONE',  ( 71.53613896966024299, 138.8348963267899592, -2.065403804986401859 ) ) ;
#11608 = ORIENTED_EDGE ( 'NONE', *, *, #17575, .T. ) ;
#11609 = CARTESIAN_POINT ( 'NONE',  ( 69.45715107853048664, 110.1171555912624740, -7.938611875467805667 ) ) ;
#11610 = ORIENTED_EDGE ( 'NONE', *, *, #13532, .F. ) ;
#11611 = CARTESIAN_POINT ( 'NONE',  ( 43.01140435219951286, 121.1297705074273097, 38.86567161673127657 ) ) ;
#11612 = CARTESIAN_POINT ( 'NONE',  ( 77.34521997529867576, 314.8592298662555322, 4.000000000000003553 ) ) ;
#11613 = CARTESIAN_POINT ( 'NONE',  ( 41.64333658814960870, 84.97977050742731819, 38.42115945441014446 ) ) ;
#11614 = CARTESIAN_POINT ( 'NONE',  ( 47.43856463449118621, 157.6151871740940180, 34.21067981925357060 ) ) ;
#11615 = CARTESIAN_POINT ( 'NONE',  ( 31.13415902118537559, 151.9291573665896635, 4.438733124005141306 ) ) ;
#11616 = CARTESIAN_POINT ( 'NONE',  ( 139.9279279298906147, 262.8829071470229906, -5.999999999999976019 ) ) ;
#11617 = CARTESIAN_POINT ( 'NONE',  ( 48.01140435219951996, 82.43445800887258201, 32.58608133808903773 ) ) ;
#11618 = CARTESIAN_POINT ( 'NONE',  ( -23.27144139456156324, -18.88988604584387332, 4.000000000000021316 ) ) ;
#11619 = CARTESIAN_POINT ( 'NONE',  ( -157.6495955161842062, -176.9391397928654897, 41.15050349809590102 ) ) ;
#11620 = CARTESIAN_POINT ( 'NONE',  ( 38.01140435219952707, 89.78445800887257633, 34.21067981925357060 ) ) ;
#11621 = DIRECTION ( 'NONE',  ( 0.000000000000000000, 1.000000000000000000, -0.000000000000000000 ) ) ;
#11622 = CARTESIAN_POINT ( 'NONE',  ( -157.2955611005346270, -194.3438272943106995, 41.63779006702063867 ) ) ;
#11623 = CARTESIAN_POINT ( 'NONE',  ( 40.27526882409969033, 92.92977050742729261, 30.44471234641811819 ) ) ;
#11624 = CARTESIAN_POINT ( 'NONE',  ( 50.58784882905466418, 147.1537178454131549, 17.22345644918840790 ) ) ;
#11625 = CARTESIAN_POINT ( 'NONE',  ( 54.85617982533816672, 239.2521282348021714, -19.99999999999996092 ) ) ;
#11626 = EDGE_LOOP ( 'NONE', ( #21266, #2759, #3589, #4257 ) ) ;
#11627 = CARTESIAN_POINT ( 'NONE',  ( -143.3790856849358306, -190.2891397928654555, 55.53486410454105027 ) ) ;
#11628 = CARTESIAN_POINT ( 'NONE',  ( 26.66797635711824199, 149.9459070286683868, 17.30505193804556185 ) ) ;
#11629 = CARTESIAN_POINT ( 'NONE',  ( 47.43856463449118621, 139.8797705074273381, 34.21067981925357060 ) ) ;
#11630 = CARTESIAN_POINT ( 'NONE',  ( 67.53959295026429288, 106.1551078129065075, 0.2323293680688409690 ) ) ;
#11631 = CARTESIAN_POINT ( 'NONE',  ( 47.43856463449117911, 65.02977050742732956, 32.77220824515697473 ) ) ;
#11632 = ORIENTED_EDGE ( 'NONE', *, *, #15940, .F. ) ;
#11633 = CARTESIAN_POINT ( 'NONE',  ( 38.58424406990784661, 141.5297705074272869, 35.64915139335016647 ) ) ;
#11634 = EDGE_CURVE ( 'NONE', #20857, #1303, #5255, .T. ) ;
#11636 = ADVANCED_FACE ( 'NONE', ( #10223, #5459 ), #8571, .T. ) ;
#11635 = CARTESIAN_POINT ( 'NONE',  ( 47.05648932407426344, 151.9104996726487400, 37.14960608071593384 ) ) ;
#11637 = CARTESIAN_POINT ( 'NONE',  ( 43.01140435219951286, 115.4604996726487229, 39.46799094044489209 ) ) ;
#11638 = CARTESIAN_POINT ( 'NONE',  ( 41.64333658814960870, 68.51518717409399528, 30.00020018409699318 ) ) ;
#11639 = DIRECTION ( 'NONE',  ( 1.000000000000000000, 0.000000000000000000, -0.000000000000000000 ) ) ;
#11640 =( BOUNDED_SURFACE ( )  B_SPLINE_SURFACE ( 1, 2, ( 
 ( #2289, #9029, #4269, #645, #10788, #9141, #15841, #17602, #4169, #12650, #10898, #9249, #859, #7595, #14294, #21039, #19926, #19702, #4592, #11311, #3277, #14946, #18264, #9683, #7917, #17922, #21801, #13416, #16380, #13311, #21693, #20047, #8244, #20151, #21357, #4934, #5043, #14620, #6592, #16599, #18036, #9792, #8353, #6361, #10007, #6248, #18375, #11644, #16486, #1403, #2941, #6472, #1292, #16712, #8132, #1621, #13084, #13193, #3168, #15064, #2832, #9571, #16277, #12978, #4814, #8027, #14734, #21470, #1183, #19813, #9897, #4702, #18146, #14835, #21581, #1515, #3503, #7137, #15505, #13841, #2060, #15602, #15177, #20577, #508, #1734, #407, #10444, #11867, #3611, #2163, #183, #18920, #79, #12185, #5463, #10334, #17037, #18599, #299, #20256, #3823, #1949, #10549, #7028, #8469, #10115, #20685, #18810, #6816, #17250, #8900, #8791, #7247, #5363, #13947, #11754, #13522, #5147, #18485, #3390, #10226, #17146, #16822, #16928, #1844, #8574, #15290, #6920, #13624, #20363, #5258, #11975, #18705, #8679, #15401, #13733, #20471, #12080, #3715, #17788, #2586, #5682, #2482, #16141, #3928, #5895, #729, #14488, #9441, #17576, #21119, #7683, #7457, #12625, #1050, #11073, #14166, #9224, #14380, #20899, #19030, #12406, #19347, #17469, #2696, #10659, #4245, #5786, #7568, #15922, #14268, #17361, #19137, #10971, #938, #6003, #7784, #21013, #5569, #9004, #7354, #12732, #12518, #19455, #4345, #19242, #17683, #12292, #2267, #4142, #834, #15715, #10875, #619, #4036, #9326, #2379, #14057, #20790, #16025, #10763, #9117, #15815, #1377, #4452, #21334, #6447, #16571, #1490, #10280, #8106, #18652, #2809, #1159, #6564, #14709, #16356, #9766, #21557, #8220, #3555, #6109, #14921, #17896, #14812, #7892, #14593, #6221, #13571, #18239, #13169, #12952, #11183, #21230, #16984, #1892, #19675, #21670, #3141, #20309, #11509, #8628, #9547, #5208, #12839, #16250, #9871, #19901, #4567, #13060, #11923, #9656, #19557, #11289, #18010, #2921, #19788, #4680, #1267, #16463, #8002, #21445, #11395, #6335, #4789, #18119, #3029, #19636, #17751, #687, #17860, #9512, #6076, #19522, #4312, #4415, #6181, #7423, #14122, #1121, #11146, #20861, #16102, #16211, #12913, #7855, #21298, #15882, #12474, #10725, #10836, #2444, #2336, #795, #17534, #9073, #9184, #7529, #11036, #14230, #5858, #12588, #19311, #7642, #4208, #10938, #2654, #17645, #2552, #9289, #21085, #15989, #5966, #12692, #19415, #4863, #9728, #6753, #11690, #11583, #6644, #8182, #19746, #4641, #6407, #4978, #14992, #14884, #18426, #11360, #4529, #13132, #19859, #16757, #4746, #18195, #3102, #1559, #1450, #1669, #8401, #18312, #13241, #13, #16534, #21630, #6521, #21736, #5301, #2205, #12232, #3865, #18963, #1990, #7290, #1882, #226, #3757, #3543, #12118, #6853, #10268, #13670, #17292, #5502, #7176, #16971, #7070, #13880, #8723, #13560, #18849, #12012, #15334, #8513, #18747, #8615, #447, #8834, #17185, #3650, #10164, #15643, #10377, #10485, #16863, #15441, #6964, #15540, #20402, #2098, #3439, #15225, #20619, #8937, #10589, #547, #20194, #5087, #124, #11801, #20296, #18532, #1779, #5193, #11911, #18640, #17078, #340, #13774, #20514, #5401, #4184, #12337, #20726, #20944, #875, #9157, #4075, #7721, #16181, #659, #16070, #5826, #14312, #3974, #19494, #12557, #983, #14422, #1094, #6044, #19285, #10913, #4281, #14205, #19071, #2307, #17617, #11118, #4386, #11011, #14098, #2523, #2743, #10697, #21057, #15858, #13989, #17832, #9263, #21158, #12772, #768, #5937, #9482, #5612, #7504, #15963, #17403, #7610, #9046, #20833, #12666, #10805, #15756, #7397, #19387, #17721, #2627, #9366, #5725, #12448, #19176, #17509, #2418, #3182, #18394, #16502, #4948, #11220, #9587, #14960, #1306, #2956, #18161, #8148, #9911, #11657, #14529, #16617, #4497, #1419, #16289, #1196, #7930, #21706, #4830, #14853, #21375, #19603, #7825, #3294, #10022, #6262, #1528, #11552, #8260, #19944, #16727, #17937, #6607, #21269, #2845, #18281, #6488, #14635, #21487, #20061, #18049, #13326, #12995, #6148, #12883, #6374, #13102, #19715, #3068, #4607, #11326, #19826, #9696, #21599, #16395, #8042, #4716, #13208, #11436, #8804, #15516, #20486, #10459, #17051, #17159, #18937, #20169, #5058, #13854, #2074, #13431, #312, #419, #3837, #5376, #7151, #6828, #3410, #7041, #11772, #15193, #15080, #13535, #6724, #13747, #10132, #12202, #1963, #8484, #15416, #20270, #20591, #18501, #8697, #18611, #3624, #13640, #10346, #16837, #1750, #12091, #18823, #3729, #10564, #5476, #1637, #97, #5161, #8369, #16940, #3516, #11987, #21816, #11882, #10241, #1855, #8586, #15305, #198, #6935, #20376, #5272, #18717, #14583, #11175, #9018, #7259, #17264, #21435, #6325, #15730, #12943, #21326, #19665, #7883, #13051, #20701, #4557, #19776, #13961, #6211, #16238, #17374, #9428, #7992, #5699, #2913, #5584, #17998, #11280, #16133, #1041, #2279, #6098, #3944, #9646, #7776, #16347, #12829, #12308, #15615, #4671, #2799, #19045, #1255, #14697, #2176, #8912, #17886, #523, #10671, #634, #7370, #14071, #20808, #12721, #1148, #19444, #4337, #11063, #17778, #2684, #14474, #21219, #19548, #4443, #9539, #16562, #16454 ),
 ( #16789, #1478, #3354, #19891, #8211, #4895, #8542, #18563, #20222, #43, #11614, #18342, #5009, #11719, #9862, #13592, #3470, #18454, #13491, #15028, #3019, #4778, #14911, #11833, #6783, #21768, #10194, #13161, #11388, #21661, #6551, #16896, #13275, #11499, #1365, #1703, #8319, #5116, #1810, #10080, #20119, #15254, #9757, #18110, #153, #20011, #3243, #6885, #20329, #8097, #14805, #6674, #21545, #9974, #16677, #8432, #1588, #15140, #18230, #13381, #6438, #3132, #12366, #14020, #2023, #13911, #20755, #15570, #13700, #3896, #12148, #372, #15367, #18880, #17109, #7321, #15674, #2235, #3788, #17002, #689, #10517, #10620, #1910, #475, #10408, #578, #5428, #8968, #10300, #260, #17328, #9076, #5646, #19105, #17431, #4001, #6996, #18996, #20435, #10730, #14125, #8646, #5227, #5329, #12047, #2339, #13807, #18777, #15783, #17213, #3574, #11942, #2128, #20649, #7101, #8755, #7426, #18671, #3679, #15472, #8863, #5532, #20545, #7209, #12261, #7858, #14559, #7963, #12916, #19418, #12696, #11149, #21088, #4105, #9187, #2657, #12592, #10840, #20864, #2882, #9621, #19314, #16214, #2776, #1125, #17862, #16320, #2447, #21301, #1229, #17537, #9516, #19526, #20974, #4315, #11252, #9292, #6185, #15885, #19640, #4532, #11039, #17755, #5862, #9400, #7532, #17973, #16109, #5751, #1017, #798, #19208, #12480, #6079, #14234, #4212, #10940, #17648, #2555, #14452, #15993, #902, #7647, #14346, #5969, #7754, #21191, #4419, #12805, #16868, #18428, #6756, #19862, #16428, #20093, #2990, #6412, #6298, #4749, #19751, #4982, #1340, #3442, #14997, #11804, #5090, #11693, #14780, #11587, #10167, #13027, #21739, #9837, #1782, #18535, #4866, #8404, #16761, #16537, #6647, #14670, #20197, #1453, #18315, #1672, #8186, #4645, #21523, #13356, #11469, #21410, #11363, #3326, #14887, #16651, #3215, #1563, #18084, #13135, #10055, #15113, #16, #9731, #8290, #8074, #18198, #3105, #13464, #21633, #6524, #9948, #13245, #19981, #12340, #15229, #3869, #5197, #10488, #10271, #16974, #1884, #15646, #5505, #2100, #2209, #10701, #8618, #10592, #15444, #8838, #20299, #13993, #345, #17297, #8940, #17405, #550, #7074, #13777, #20622, #8726, #13563, #18644, #12120, #18966, #1995, #20516, #15544, #449, #6967, #8516, #7294, #7179, #20729, #18853, #127, #15337, #13673, #5617, #19075, #3761, #3976, #229, #6856, #20406, #18750, #11914, #3653, #5304, #3546, #13883, #5403, #12016, #10381, #12235, #17188, #17081, #15758, #9049, #11121, #4187, #9265, #6151, #16184, #7830, #1096, #5940, #11223, #5828, #10915, #7724, #7507, #16075, #10809, #14207, #17621, #21273, #9485, #17836, #20946, #11014, #2746, #12670, #17512, #986, #15965, #19288, #12452, #877, #12561, #4389, #12776, #21161, #7614, #14101, #19607, #14316, #14426, #20837, #19390, #2529, #19497, #21059, #6050, #7400, #19180, #14532, #12886, #4500, #2310, #663, #5728, #4079, #2421, #9161, #15860, #773, #4287, #17725, #2630, #9370, #15083, #4719, #11331, #10025, #8151, #16293, #2848, #3072, #4833, #13106, #8045, #18661, #3297, #4952, #14750, #11556, #11660, #6491, #4610, #16621, #9810, #19829, #6265, #16505, #21491, #20065, #6613, #14963, #1422, #7934, #13434, #14856, #1531, #14638, #13211, #1310, #13329, #18164, #21710, #1199, #12998, #8263, #6728, #18397, #16730, #8373, #1640, #19719, #9914, #18052, #20172, #5062, #21379, #17942, #2960, #9699, #9592, #11439, #16399, #6377, #21602, #19948, #18284, #3186, #20489, #6938, #1859, #5480, #13964, #20273, #13857, #18720, #12094, #1753, #17268, #3627, #20594, #12205, #20704, #3840, #10351, #17054, #2077, #11990, #16840, #100, #15420, #422, #5275, #1966, #5379, #18827, #10245, #11775, #18940, #3732, #10567, #316, #3413, #5165, #16943, #2179, #7154, #7044, #8915, #13538, #18504, #8589, #200, #15618, #13645, #11886, #8488, #17163, #8699, #526, #7263, #10462, #8808, #10136, #15197, #6831, #18614, #20379, #13750, #3519, #15308, #15519, #4364, #9243, #14507, #9134, #7480, #10991, #10781, #19365, #14074, #17487, #20920, #17377, #852, #2397, #958, #5803, #2606, #10674, #15733, #4263, #9458, #21137, #7701, #17806, #9344, #7373, #17701, #20812, #14399, #5587, #2282, #12312, #5702, #12426, #2717, #14182, #19152, #19472, #17595, #3948, #19048, #12534, #14288, #745, #15834, #6021, #7801, #4053, #12752, #19261, #5915, #9022, #11094, #4163, #16159, #1071, #638, #10892, #2501, #15942, #16047, #7588, #21032, #12644, #3048, #9891, #14727, #6354, #14829, #21574, #19696, #1615, #6585, #6465, #1509, #9785, #12857, #14614, #4584, #21687, #16591, #16481, #13303, #1175, #21249, #11304, #9674, #20041, #16374, #7911, #4471, #4808, #18139, #8238, #11638, #13186, #8126, #14940, #11201, #6127, #4927, #1287, #13078, #3270, #18368, #10002, #16706, #1397, #8347, #2937, #8022, #11530, #18031, #19919, #21352, #21463, #19807, #17914, #9564, #16269, #4696, #18258, #6241, #3161, #12970, #11413, #177, #10221, #3383, #6912, #5142, #17137, #3706, #12071, #13618, #5038, #10542, #20356, #20462, #10436, #15282, #18801, #20145, #10109, #13726, #18910, #8784, #2051, #5455, #15497, #16816, #7022, #8463, #399, #2156, #11747, #15058, #15170, #73 ) ),
 .UNSPECIFIED., .F., .F., .F. ) 
 B_SPLINE_SURFACE_WITH_KNOTS ( ( 2, 2 ),
 ( 3, 2, 2, 2, 2, 2, 2, 2, 2, 2, 2, 2, 2, 2, 2, 2, 2, 2, 2, 2, 2, 2, 2, 2, 2, 2, 2, 2, 2, 2, 2, 2, 2, 2, 2, 2, 2, 2, 2, 2, 2, 2, 2, 2, 2, 2, 2, 2, 2, 2, 2, 2, 2, 2, 2, 2, 2, 2, 2, 2, 2, 2, 2, 2, 2, 2, 2, 2, 2, 2, 2, 2, 2, 2, 2, 2, 2, 2, 2, 2, 2, 2, 2, 2, 2, 2, 2, 2, 2, 2, 2, 2, 2, 2, 2, 2, 2, 2, 2, 2, 2, 2, 2, 2, 2, 2, 2, 2, 2, 2, 2, 2, 2, 2, 2, 2, 2, 2, 2, 2, 2, 2, 2, 2, 2, 2, 2, 2, 2, 2, 2, 2, 2, 2, 2, 2, 2, 2, 2, 2, 2, 2, 2, 2, 2, 2, 2, 2, 2, 2, 2, 2, 2, 2, 2, 2, 2, 2, 2, 2, 2, 2, 2, 2, 2, 2, 2, 2, 2, 2, 2, 2, 2, 2, 2, 2, 2, 2, 2, 2, 2, 2, 2, 2, 2, 2, 2, 2, 2, 2, 2, 2, 2, 2, 2, 2, 2, 2, 2, 2, 2, 2, 2, 2, 2, 2, 2, 2, 2, 2, 2, 2, 2, 2, 2, 2, 2, 2, 2, 2, 2, 2, 2, 2, 2, 2, 2, 2, 2, 2, 2, 2, 2, 2, 2, 2, 2, 2, 2, 2, 2, 2, 2, 2, 2, 2, 2, 2, 2, 2, 2, 2, 2, 2, 2, 2, 2, 2, 2, 2, 2, 2, 2, 2, 2, 2, 2, 2, 2, 2, 2, 2, 2, 2, 2, 2, 2, 2, 2, 2, 2, 2, 2, 2, 2, 2, 2, 2, 2, 2, 2, 2, 2, 2, 2, 2, 2, 2, 2, 2, 2, 2, 2, 2, 2, 2, 2, 2, 2, 2, 2, 2, 2, 2, 2, 2, 2, 2, 2, 2, 2, 2, 2, 2, 2, 2, 2, 2, 2, 2, 2, 2, 2, 2, 3 ),
 ( 0.000000000000000000, 1.000000000000000000 ),
 ( 0.000000000000000000, 0.002941176470588235253, 0.005882352941176470507, 0.008823529411764705760, 0.01176470588235294101, 0.01470588235294117627, 0.01764705882352941152, 0.02058823529411764677, 0.02352941176470588203, 0.02647058823529411728, 0.02941176470588235253, 0.03235294117647059126, 0.03529411764705882304, 0.03823529411764706176, 0.04117647058823529355, 0.04411764705882353227, 0.04705882352941176405, 0.05000000000000000278, 0.05294117647058823456, 0.05588235294117647328, 0.05882352941176470507, 0.06176470588235294379, 0.06470588235294118251, 0.06764705882352940736, 0.07058823529411764608, 0.07352941176470588480, 0.07647058823529412352, 0.07941176470588234837, 0.08235294117647058709, 0.08529411764705882582, 0.08823529411764706454, 0.09117647058823528938, 0.09411764705882352811, 0.09705882352941176683, 0.1000000000000000056, 0.1029411764705882304, 0.1058823529411764691, 0.1088235294117647078, 0.1117647058823529466, 0.1147058823529411714, 0.1176470588235294101, 0.1205882352941176489, 0.1235294117647058876, 0.1264705882352941124, 0.1294117647058823650, 0.1323529411764705899, 0.1352941176470588147, 0.1382352941176470673, 0.1411764705882352922, 0.1441176470588235170, 0.1470588235294117696, 0.1499999999999999944, 0.1529411764705882470, 0.1558823529411764719, 0.1588235294117646967, 0.1617647058823529493, 0.1647058823529411742, 0.1676470588235293990, 0.1705882352941176516, 0.1735294117647058765, 0.1764705882352941291, 0.1794117647058823539, 0.1823529411764705788, 0.1852941176470588314, 0.1882352941176470562, 0.1911764705882352811, 0.1941176470588235337, 0.1970588235294117585, 0.2000000000000000111, 0.2029411764705882359, 0.2058823529411764608, 0.2088235294117647134, 0.2117647058823529382, 0.2147058823529411631, 0.2176470588235294157, 0.2205882352941176405, 0.2235294117647058931, 0.2264705882352941180, 0.2294117647058823428, 0.2323529411764705954, 0.2352941176470588203, 0.2382352941176470451, 0.2411764705882352977, 0.2441176470588235226, 0.2470588235294117752, 0.2500000000000000000, 0.2529411764705882248, 0.2558823529411764497, 0.2588235294117647300, 0.2617647058823529549, 0.2647058823529411797, 0.2676470588235294046, 0.2705882352941176294, 0.2735294117647059098, 0.2764705882352941346, 0.2794117647058823595, 0.2823529411764705843, 0.2852941176470588092, 0.2882352941176470340, 0.2911764705882353144, 0.2941176470588235392, 0.2970588235294117641, 0.2999999999999999889, 0.3029411764705882137, 0.3058823529411764941, 0.3088235294117647189, 0.3117647058823529438, 0.3147058823529411686, 0.3176470588235293935, 0.3205882352941176738, 0.3235294117647058987, 0.3264705882352941235, 0.3294117647058823484, 0.3323529411764705732, 0.3352941176470587981, 0.3382352941176470784, 0.3411764705882353033, 0.3441176470588235281, 0.3470588235294117530, 0.3499999999999999778, 0.3529411764705882582, 0.3558823529411764830, 0.3588235294117647078, 0.3617647058823529327, 0.3647058823529411575, 0.3676470588235294379, 0.3705882352941176627, 0.3735294117647058876, 0.3764705882352941124, 0.3794117647058823373, 0.3823529411764705621, 0.3852941176470588425, 0.3882352941176470673, 0.3911764705882352922, 0.3941176470588235170, 0.3970588235294117418, 0.4000000000000000222, 0.4029411764705882470, 0.4058823529411764719, 0.4088235294117646967, 0.4117647058823529216, 0.4147058823529412019, 0.4176470588235294268, 0.4205882352941176516, 0.4235294117647058765, 0.4264705882352941013, 0.4294117647058823262, 0.4323529411764706065, 0.4352941176470588314, 0.4382352941176470562, 0.4411764705882352811, 0.4441176470588235059, 0.4470588235294117863, 0.4500000000000000111, 0.4529411764705882359, 0.4558823529411764608, 0.4588235294117646856, 0.4617647058823529660, 0.4647058823529411908, 0.4676470588235294157, 0.4705882352941176405, 0.4735294117647058654, 0.4764705882352940902, 0.4794117647058823706, 0.4823529411764705954, 0.4852941176470588203, 0.4882352941176470451, 0.4911764705882352700, 0.4941176470588235503, 0.4970588235294117752, 0.5000000000000000000, 0.5029411764705882248, 0.5058823529411764497, 0.5088235294117646745, 0.5117647058823528994, 0.5147058823529411242, 0.5176470588235294601, 0.5205882352941176849, 0.5235294117647059098, 0.5264705882352941346, 0.5294117647058823595, 0.5323529411764705843, 0.5352941176470588092, 0.5382352941176470340, 0.5411764705882352589, 0.5441176470588234837, 0.5470588235294118196, 0.5500000000000000444, 0.5529411764705882693, 0.5558823529411764941, 0.5588235294117647189, 0.5617647058823529438, 0.5647058823529411686, 0.5676470588235293935, 0.5705882352941176183, 0.5735294117647058432, 0.5764705882352940680, 0.5794117647058824039, 0.5823529411764706287, 0.5852941176470588536, 0.5882352941176470784, 0.5911764705882353033, 0.5941176470588235281, 0.5970588235294117530, 0.5999999999999999778, 0.6029411764705882026, 0.6058823529411764275, 0.6088235294117646523, 0.6117647058823529882, 0.6147058823529412130, 0.6176470588235294379, 0.6205882352941176627, 0.6235294117647058876, 0.6264705882352941124, 0.6294117647058823373, 0.6323529411764705621, 0.6352941176470587870, 0.6382352941176470118, 0.6411764705882353477, 0.6441176470588235725, 0.6470588235294117974, 0.6500000000000000222, 0.6529411764705882470, 0.6558823529411764719, 0.6588235294117646967, 0.6617647058823529216, 0.6647058823529411464, 0.6676470588235293713, 0.6705882352941175961, 0.6735294117647059320, 0.6764705882352941568, 0.6794117647058823817, 0.6823529411764706065, 0.6852941176470588314, 0.6882352941176470562, 0.6911764705882352811, 0.6941176470588235059, 0.6970588235294117307, 0.6999999999999999556, 0.7029411764705881804, 0.7058823529411765163, 0.7088235294117647411, 0.7117647058823529660, 0.7147058823529411908, 0.7176470588235294157, 0.7205882352941176405, 0.7235294117647058654, 0.7264705882352940902, 0.7294117647058823151, 0.7323529411764705399, 0.7352941176470588758, 0.7382352941176471006, 0.7411764705882353255, 0.7441176470588235503, 0.7470588235294117752, 0.7500000000000000000, 0.7529411764705882248, 0.7558823529411764497, 0.7588235294117646745, 0.7617647058823528994, 0.7647058823529411242, 0.7676470588235294601, 0.7705882352941176849, 0.7735294117647059098, 0.7764705882352941346, 0.7794117647058823595, 0.7823529411764705843, 0.7852941176470588092, 0.7882352941176470340, 0.7911764705882352589, 0.7941176470588234837, 0.7970588235294118196, 0.8000000000000000444, 0.8029411764705882693, 0.8058823529411764941, 0.8088235294117647189, 0.8117647058823529438, 0.8147058823529411686, 0.8176470588235293935, 0.8205882352941176183, 0.8235294117647058432, 0.8264705882352940680, 0.8294117647058824039, 0.8323529411764706287, 0.8352941176470588536, 0.8382352941176470784, 0.8411764705882353033, 0.8441176470588235281, 0.8470588235294117530, 0.8499999999999999778, 0.8529411764705882026, 0.8558823529411764275, 0.8588235294117646523, 0.8617647058823529882, 0.8647058823529412130, 0.8676470588235294379, 0.8705882352941176627, 0.8735294117647058876, 0.8764705882352941124, 0.8794117647058823373, 0.8823529411764705621, 0.8852941176470587870, 0.8882352941176470118, 0.8911764705882353477, 0.8941176470588235725, 0.8970588235294117974, 0.9000000000000000222, 0.9029411764705882470, 0.9058823529411764719, 0.9088235294117646967, 0.9117647058823529216, 0.9147058823529411464, 0.9176470588235293713, 0.9205882352941175961, 0.9235294117647059320, 0.9264705882352941568, 0.9294117647058823817, 0.9323529411764706065, 0.9352941176470588314, 0.9382352941176470562, 0.9411764705882352811, 0.9441176470588235059, 0.9470588235294117307, 0.9499999999999999556, 0.9529411764705881804, 0.9558823529411765163, 0.9588235294117647411, 0.9617647058823529660, 0.9647058823529411908, 0.9676470588235294157, 0.9705882352941176405, 0.9735294117647058654, 0.9764705882352940902, 0.9794117647058823151, 0.9803958162805426202 ),
 .UNSPECIFIED. ) 
 GEOMETRIC_REPRESENTATION_ITEM ( )  RATIONAL_B_SPLINE_SURFACE ( (
 ( 1.000000000000000000, 0.9510565162951535312, 1.000000000000000000, 0.9510565162951535312, 1.000000000000000000, 0.9510565162951535312, 1.000000000000000000, 0.9510565162951535312, 1.000000000000000000, 0.9510565162951535312, 1.000000000000000000, 0.9510565162951535312, 1.000000000000000000, 0.9510565162951535312, 1.000000000000000000, 0.9510565162951535312, 1.000000000000000000, 0.9510565162951535312, 1.000000000000000000, 0.9510565162951535312, 1.000000000000000000, 0.9510565162951535312, 1.000000000000000000, 0.9510565162951535312, 1.000000000000000000, 0.9510565162951535312, 1.000000000000000000, 0.9510565162951535312, 1.000000000000000000, 0.9510565162951535312, 1.000000000000000000, 0.9510565162951535312, 1.000000000000000000, 0.9510565162951535312, 1.000000000000000000, 0.9510565162951535312, 1.000000000000000000, 0.9510565162951535312, 1.000000000000000000, 0.9510565162951535312, 1.000000000000000000, 0.9510565162951535312, 1.000000000000000000, 0.9510565162951535312, 1.000000000000000000, 0.9510565162951535312, 1.000000000000000000, 0.9510565162951535312, 1.000000000000000000, 0.9510565162951535312, 1.000000000000000000, 0.9510565162951535312, 1.000000000000000000, 0.9510565162951535312, 1.000000000000000000, 0.9510565162951535312, 1.000000000000000000, 0.9510565162951535312, 1.000000000000000000, 0.9510565162951535312, 1.000000000000000000, 0.9510565162951535312, 1.000000000000000000, 0.9510565162951535312, 1.000000000000000000, 0.9510565162951535312, 1.000000000000000000, 0.9510565162951535312, 1.000000000000000000, 0.9510565162951535312, 1.000000000000000000, 0.9510565162951535312, 1.000000000000000000, 0.9510565162951535312, 1.000000000000000000, 0.9510565162951535312, 1.000000000000000000, 0.9510565162951535312, 1.000000000000000000, 0.9510565162951535312, 1.000000000000000000, 0.9510565162951535312, 1.000000000000000000, 0.9510565162951535312, 1.000000000000000000, 0.9510565162951535312, 1.000000000000000000, 0.9510565162951535312, 1.000000000000000000, 0.9510565162951535312, 1.000000000000000000, 0.9510565162951535312, 1.000000000000000000, 0.9510565162951535312, 1.000000000000000000, 0.9510565162951535312, 1.000000000000000000, 0.9510565162951535312, 1.000000000000000000, 0.9510565162951535312, 1.000000000000000000, 0.9510565162951535312, 1.000000000000000000, 0.9510565162951535312, 1.000000000000000000, 0.9510565162951535312, 1.000000000000000000, 0.9510565162951535312, 1.000000000000000000, 0.9510565162951535312, 1.000000000000000000, 0.9510565162951535312, 1.000000000000000000, 0.9510565162951535312, 1.000000000000000000, 0.9510565162951535312, 1.000000000000000000, 0.9510565162951535312, 1.000000000000000000, 0.9510565162951535312, 1.000000000000000000, 0.9510565162951535312, 1.000000000000000000, 0.9510565162951535312, 1.000000000000000000, 0.9510565162951535312, 1.000000000000000000, 0.9510565162951535312, 1.000000000000000000, 0.9510565162951535312, 1.000000000000000000, 0.9510565162951535312, 1.000000000000000000, 0.9510565162951535312, 1.000000000000000000, 0.9510565162951535312, 1.000000000000000000, 0.9510565162951535312, 1.000000000000000000, 0.9510565162951535312, 1.000000000000000000, 0.9510565162951535312, 1.000000000000000000, 0.9510565162951535312, 1.000000000000000000, 0.9510565162951535312, 1.000000000000000000, 0.9510565162951535312, 1.000000000000000000, 0.9510565162951535312, 1.000000000000000000, 0.9510565162951535312, 1.000000000000000000, 0.9510565162951535312, 1.000000000000000000, 0.9510565162951535312, 1.000000000000000000, 0.9510565162951535312, 1.000000000000000000, 0.9510565162951535312, 1.000000000000000000, 0.9510565162951535312, 1.000000000000000000, 0.9510565162951535312, 1.000000000000000000, 0.9510565162951535312, 1.000000000000000000, 0.9510565162951535312, 1.000000000000000000, 0.9510565162951535312, 1.000000000000000000, 0.9510565162951535312, 1.000000000000000000, 0.9510565162951535312, 1.000000000000000000, 0.9510565162951535312, 1.000000000000000000, 0.9510565162951535312, 1.000000000000000000, 0.9510565162951535312, 1.000000000000000000, 0.9510565162951535312, 1.000000000000000000, 0.9510565162951535312, 1.000000000000000000, 0.9510565162951535312, 1.000000000000000000, 0.9510565162951535312, 1.000000000000000000, 0.9510565162951535312, 1.000000000000000000, 0.9510565162951535312, 1.000000000000000000, 0.9510565162951535312, 1.000000000000000000, 0.9510565162951535312, 1.000000000000000000, 0.9510565162951535312, 1.000000000000000000, 0.9510565162951535312, 1.000000000000000000, 0.9510565162951535312, 1.000000000000000000, 0.9510565162951535312, 1.000000000000000000, 0.9510565162951535312, 1.000000000000000000, 0.9510565162951535312, 1.000000000000000000, 0.9510565162951535312, 1.000000000000000000, 0.9510565162951535312, 1.000000000000000000, 0.9510565162951535312, 1.000000000000000000, 0.9510565162951535312, 1.000000000000000000, 0.9510565162951535312, 1.000000000000000000, 0.9510565162951535312, 1.000000000000000000, 0.9510565162951535312, 1.000000000000000000, 0.9510565162951535312, 1.000000000000000000, 0.9510565162951535312, 1.000000000000000000, 0.9510565162951535312, 1.000000000000000000, 0.9510565162951535312, 1.000000000000000000, 0.9510565162951535312, 1.000000000000000000, 0.9510565162951535312, 1.000000000000000000, 0.9510565162951535312, 1.000000000000000000, 0.9510565162951535312, 1.000000000000000000, 0.9510565162951535312, 1.000000000000000000, 0.9510565162951535312, 1.000000000000000000, 0.9510565162951535312, 1.000000000000000000, 0.9510565162951535312, 1.000000000000000000, 0.9510565162951535312, 1.000000000000000000, 0.9510565162951535312, 1.000000000000000000, 0.9510565162951535312, 1.000000000000000000, 0.9510565162951535312, 1.000000000000000000, 0.9510565162951535312, 1.000000000000000000, 0.9510565162951535312, 1.000000000000000000, 0.9510565162951535312, 1.000000000000000000, 0.9510565162951535312, 1.000000000000000000, 0.9510565162951535312, 1.000000000000000000, 0.9510565162951535312, 1.000000000000000000, 0.9510565162951535312, 1.000000000000000000, 0.9510565162951535312, 1.000000000000000000, 0.9510565162951535312, 1.000000000000000000, 0.9510565162951535312, 1.000000000000000000, 0.9510565162951535312, 1.000000000000000000, 0.9510565162951535312, 1.000000000000000000, 0.9510565162951535312, 1.000000000000000000, 0.9510565162951535312, 1.000000000000000000, 0.9510565162951535312, 1.000000000000000000, 0.9510565162951535312, 1.000000000000000000, 0.9510565162951535312, 1.000000000000000000, 0.9510565162951535312, 1.000000000000000000, 0.9510565162951535312, 1.000000000000000000, 0.9510565162951535312, 1.000000000000000000, 0.9510565162951535312, 1.000000000000000000, 0.9510565162951535312, 1.000000000000000000, 0.9510565162951535312, 1.000000000000000000, 0.9510565162951535312, 1.000000000000000000, 0.9510565162951535312, 1.000000000000000000, 0.9510565162951535312, 1.000000000000000000, 0.9510565162951535312, 1.000000000000000000, 0.9510565162951535312, 1.000000000000000000, 0.9510565162951535312, 1.000000000000000000, 0.9510565162951535312, 1.000000000000000000, 0.9510565162951535312, 1.000000000000000000, 0.9510565162951535312, 1.000000000000000000, 0.9510565162951535312, 1.000000000000000000, 0.9510565162951535312, 1.000000000000000000, 0.9510565162951535312, 1.000000000000000000, 0.9510565162951535312, 1.000000000000000000, 0.9510565162951535312, 1.000000000000000000, 0.9510565162951535312, 1.000000000000000000, 0.9510565162951535312, 1.000000000000000000, 0.9510565162951535312, 1.000000000000000000, 0.9510565162951535312, 1.000000000000000000, 0.9510565162951535312, 1.000000000000000000, 0.9510565162951535312, 1.000000000000000000, 0.9510565162951535312, 1.000000000000000000, 0.9510565162951535312, 1.000000000000000000, 0.9510565162951535312, 1.000000000000000000, 0.9510565162951535312, 1.000000000000000000, 0.9510565162951535312, 1.000000000000000000, 0.9510565162951535312, 1.000000000000000000, 0.9510565162951535312, 1.000000000000000000, 0.9510565162951535312, 1.000000000000000000, 0.9510565162951535312, 1.000000000000000000, 0.9510565162951535312, 1.000000000000000000, 0.9510565162951535312, 1.000000000000000000, 0.9510565162951535312, 1.000000000000000000, 0.9510565162951535312, 1.000000000000000000, 0.9510565162951535312, 1.000000000000000000, 0.9510565162951535312, 1.000000000000000000, 0.9510565162951535312, 1.000000000000000000, 0.9510565162951535312, 1.000000000000000000, 0.9510565162951535312, 1.000000000000000000, 0.9510565162951535312, 1.000000000000000000, 0.9510565162951535312, 1.000000000000000000, 0.9510565162951535312, 1.000000000000000000, 0.9510565162951535312, 1.000000000000000000, 0.9510565162951535312, 1.000000000000000000, 0.9510565162951535312, 1.000000000000000000, 0.9510565162951535312, 1.000000000000000000, 0.9510565162951535312, 1.000000000000000000, 0.9510565162951535312, 1.000000000000000000, 0.9510565162951535312, 1.000000000000000000, 0.9510565162951535312, 1.000000000000000000, 0.9510565162951535312, 1.000000000000000000, 0.9510565162951535312, 1.000000000000000000, 0.9510565162951535312, 1.000000000000000000, 0.9510565162951535312, 1.000000000000000000, 0.9510565162951535312, 1.000000000000000000, 0.9510565162951535312, 1.000000000000000000, 0.9510565162951535312, 1.000000000000000000, 0.9510565162951535312, 1.000000000000000000, 0.9510565162951535312, 1.000000000000000000, 0.9510565162951535312, 1.000000000000000000, 0.9510565162951535312, 1.000000000000000000, 0.9510565162951535312, 1.000000000000000000, 0.9510565162951535312, 1.000000000000000000, 0.9510565162951535312, 1.000000000000000000, 0.9510565162951535312, 1.000000000000000000, 0.9510565162951535312, 1.000000000000000000, 0.9510565162951535312, 1.000000000000000000, 0.9510565162951535312, 1.000000000000000000, 0.9510565162951535312, 1.000000000000000000, 0.9510565162951535312, 1.000000000000000000, 0.9510565162951535312, 1.000000000000000000, 0.9510565162951535312, 1.000000000000000000, 0.9510565162951535312, 1.000000000000000000, 0.9510565162951535312, 1.000000000000000000, 0.9510565162951535312, 1.000000000000000000, 0.9510565162951535312, 1.000000000000000000, 0.9510565162951535312, 1.000000000000000000, 0.9510565162951535312, 1.000000000000000000, 0.9510565162951535312, 1.000000000000000000, 0.9510565162951535312, 1.000000000000000000, 0.9510565162951535312, 1.000000000000000000, 0.9510565162951535312, 1.000000000000000000, 0.9510565162951535312, 1.000000000000000000, 0.9510565162951535312, 1.000000000000000000, 0.9510565162951535312, 1.000000000000000000, 0.9510565162951535312, 1.000000000000000000, 0.9510565162951535312, 1.000000000000000000, 0.9510565162951535312, 1.000000000000000000, 0.9510565162951535312, 1.000000000000000000, 0.9510565162951535312, 1.000000000000000000, 0.9510565162951535312, 1.000000000000000000, 0.9510565162951535312, 1.000000000000000000, 0.9510565162951535312, 1.000000000000000000, 0.9510565162951535312, 1.000000000000000000, 0.9510565162951535312, 1.000000000000000000, 0.9510565162951535312, 1.000000000000000000, 0.9510565162951535312, 1.000000000000000000, 0.9510565162951535312, 1.000000000000000000, 0.9510565162951535312, 1.000000000000000000, 0.9510565162951535312, 1.000000000000000000, 0.9510565162951535312, 1.000000000000000000, 0.9510565162951535312, 1.000000000000000000, 0.9510565162951535312, 1.000000000000000000, 0.9510565162951535312, 1.000000000000000000, 0.9510565162951535312, 1.000000000000000000, 0.9510565162951535312, 1.000000000000000000, 0.9510565162951535312, 1.000000000000000000, 0.9510565162951535312, 1.000000000000000000, 0.9510565162951535312, 1.000000000000000000, 0.9510565162951535312, 1.000000000000000000, 0.9510565162951535312, 1.000000000000000000, 0.9510565162951535312, 1.000000000000000000, 0.9510565162951535312, 1.000000000000000000, 0.9510565162951535312, 1.000000000000000000, 0.9510565162951535312, 1.000000000000000000, 0.9510565162951535312, 1.000000000000000000, 0.9510565162951535312, 1.000000000000000000, 0.9510565162951535312, 1.000000000000000000, 0.9510565162951535312, 1.000000000000000000, 0.9510565162951535312, 1.000000000000000000, 0.9510565162951535312, 1.000000000000000000, 0.9510565162951535312, 1.000000000000000000, 0.9510565162951535312, 1.000000000000000000, 0.9510565162951535312, 1.000000000000000000, 0.9510565162951535312, 1.000000000000000000, 0.9510565162951535312, 1.000000000000000000, 0.9510565162951535312, 1.000000000000000000, 0.9510565162951535312, 1.000000000000000000, 0.9510565162951535312, 1.000000000000000000, 0.9510565162951535312, 1.000000000000000000, 0.9510565162951535312, 1.000000000000000000, 0.9510565162951535312, 1.000000000000000000, 0.9510565162951535312, 1.000000000000000000, 0.9510565162951535312, 1.000000000000000000, 0.9510565162951535312, 1.000000000000000000, 0.9510565162951535312, 1.000000000000000000, 0.9510565162951535312, 1.000000000000000000, 0.9510565162951535312, 1.000000000000000000, 0.9510565162951535312, 1.000000000000000000, 0.9510565162951535312, 1.000000000000000000, 0.9510565162951535312, 1.000000000000000000, 0.9510565162951535312, 1.000000000000000000, 0.9510565162951535312, 1.000000000000000000, 0.9510565162951535312, 1.000000000000000000, 0.9510565162951535312, 1.000000000000000000, 0.9510565162951535312, 1.000000000000000000, 0.9510565162951535312, 1.000000000000000000, 0.9510565162951535312, 1.000000000000000000, 0.9510565162951535312, 1.000000000000000000, 0.9510565162951535312, 1.000000000000000000, 0.9510565162951535312, 1.000000000000000000, 0.9510565162951535312, 1.000000000000000000, 0.9510565162951535312, 1.000000000000000000, 0.9510565162951535312, 1.000000000000000000, 0.9510565162951535312, 1.000000000000000000, 0.9510565162951535312, 1.000000000000000000, 0.9510565162951535312, 1.000000000000000000, 0.9510565162951535312, 1.000000000000000000, 0.9510565162951535312, 1.000000000000000000, 0.9510565162951535312, 1.000000000000000000, 0.9510565162951535312, 1.000000000000000000, 0.9510565162951535312, 1.000000000000000000, 0.9510565162951535312, 1.000000000000000000, 0.9510565162951535312, 1.000000000000000000, 0.9510565162951535312, 1.000000000000000000, 0.9510565162951535312, 1.000000000000000000, 0.9510565162951535312, 1.000000000000000000, 0.9510565162951535312, 1.000000000000000000, 0.9510565162951535312, 1.000000000000000000, 0.9510565162951535312, 1.000000000000000000, 0.9510565162951535312, 1.000000000000000000, 0.9510565162951535312, 1.000000000000000000, 0.9510565162951535312, 1.000000000000000000, 0.9510565162951535312, 1.000000000000000000, 0.9510565162951535312, 1.000000000000000000, 0.9510565162951535312, 1.000000000000000000, 0.9510565162951535312, 1.000000000000000000, 0.9510565162951535312, 1.000000000000000000, 0.9510565162951535312, 1.000000000000000000, 0.9510565162951535312, 1.000000000000000000, 0.9510565162951535312, 1.000000000000000000, 0.9510565162951535312, 1.000000000000000000, 0.9510565162951535312, 1.000000000000000000, 0.9510565162951535312, 1.000000000000000000, 0.9836246098489007661, 0.9782068950532306628),
 ( 1.000000000000000000, 0.9510565162951535312, 1.000000000000000000, 0.9510565162951535312, 1.000000000000000000, 0.9510565162951535312, 1.000000000000000000, 0.9510565162951535312, 1.000000000000000000, 0.9510565162951535312, 1.000000000000000000, 0.9510565162951535312, 1.000000000000000000, 0.9510565162951535312, 1.000000000000000000, 0.9510565162951535312, 1.000000000000000000, 0.9510565162951535312, 1.000000000000000000, 0.9510565162951535312, 1.000000000000000000, 0.9510565162951535312, 1.000000000000000000, 0.9510565162951535312, 1.000000000000000000, 0.9510565162951535312, 1.000000000000000000, 0.9510565162951535312, 1.000000000000000000, 0.9510565162951535312, 1.000000000000000000, 0.9510565162951535312, 1.000000000000000000, 0.9510565162951535312, 1.000000000000000000, 0.9510565162951535312, 1.000000000000000000, 0.9510565162951535312, 1.000000000000000000, 0.9510565162951535312, 1.000000000000000000, 0.9510565162951535312, 1.000000000000000000, 0.9510565162951535312, 1.000000000000000000, 0.9510565162951535312, 1.000000000000000000, 0.9510565162951535312, 1.000000000000000000, 0.9510565162951535312, 1.000000000000000000, 0.9510565162951535312, 1.000000000000000000, 0.9510565162951535312, 1.000000000000000000, 0.9510565162951535312, 1.000000000000000000, 0.9510565162951535312, 1.000000000000000000, 0.9510565162951535312, 1.000000000000000000, 0.9510565162951535312, 1.000000000000000000, 0.9510565162951535312, 1.000000000000000000, 0.9510565162951535312, 1.000000000000000000, 0.9510565162951535312, 1.000000000000000000, 0.9510565162951535312, 1.000000000000000000, 0.9510565162951535312, 1.000000000000000000, 0.9510565162951535312, 1.000000000000000000, 0.9510565162951535312, 1.000000000000000000, 0.9510565162951535312, 1.000000000000000000, 0.9510565162951535312, 1.000000000000000000, 0.9510565162951535312, 1.000000000000000000, 0.9510565162951535312, 1.000000000000000000, 0.9510565162951535312, 1.000000000000000000, 0.9510565162951535312, 1.000000000000000000, 0.9510565162951535312, 1.000000000000000000, 0.9510565162951535312, 1.000000000000000000, 0.9510565162951535312, 1.000000000000000000, 0.9510565162951535312, 1.000000000000000000, 0.9510565162951535312, 1.000000000000000000, 0.9510565162951535312, 1.000000000000000000, 0.9510565162951535312, 1.000000000000000000, 0.9510565162951535312, 1.000000000000000000, 0.9510565162951535312, 1.000000000000000000, 0.9510565162951535312, 1.000000000000000000, 0.9510565162951535312, 1.000000000000000000, 0.9510565162951535312, 1.000000000000000000, 0.9510565162951535312, 1.000000000000000000, 0.9510565162951535312, 1.000000000000000000, 0.9510565162951535312, 1.000000000000000000, 0.9510565162951535312, 1.000000000000000000, 0.9510565162951535312, 1.000000000000000000, 0.9510565162951535312, 1.000000000000000000, 0.9510565162951535312, 1.000000000000000000, 0.9510565162951535312, 1.000000000000000000, 0.9510565162951535312, 1.000000000000000000, 0.9510565162951535312, 1.000000000000000000, 0.9510565162951535312, 1.000000000000000000, 0.9510565162951535312, 1.000000000000000000, 0.9510565162951535312, 1.000000000000000000, 0.9510565162951535312, 1.000000000000000000, 0.9510565162951535312, 1.000000000000000000, 0.9510565162951535312, 1.000000000000000000, 0.9510565162951535312, 1.000000000000000000, 0.9510565162951535312, 1.000000000000000000, 0.9510565162951535312, 1.000000000000000000, 0.9510565162951535312, 1.000000000000000000, 0.9510565162951535312, 1.000000000000000000, 0.9510565162951535312, 1.000000000000000000, 0.9510565162951535312, 1.000000000000000000, 0.9510565162951535312, 1.000000000000000000, 0.9510565162951535312, 1.000000000000000000, 0.9510565162951535312, 1.000000000000000000, 0.9510565162951535312, 1.000000000000000000, 0.9510565162951535312, 1.000000000000000000, 0.9510565162951535312, 1.000000000000000000, 0.9510565162951535312, 1.000000000000000000, 0.9510565162951535312, 1.000000000000000000, 0.9510565162951535312, 1.000000000000000000, 0.9510565162951535312, 1.000000000000000000, 0.9510565162951535312, 1.000000000000000000, 0.9510565162951535312, 1.000000000000000000, 0.9510565162951535312, 1.000000000000000000, 0.9510565162951535312, 1.000000000000000000, 0.9510565162951535312, 1.000000000000000000, 0.9510565162951535312, 1.000000000000000000, 0.9510565162951535312, 1.000000000000000000, 0.9510565162951535312, 1.000000000000000000, 0.9510565162951535312, 1.000000000000000000, 0.9510565162951535312, 1.000000000000000000, 0.9510565162951535312, 1.000000000000000000, 0.9510565162951535312, 1.000000000000000000, 0.9510565162951535312, 1.000000000000000000, 0.9510565162951535312, 1.000000000000000000, 0.9510565162951535312, 1.000000000000000000, 0.9510565162951535312, 1.000000000000000000, 0.9510565162951535312, 1.000000000000000000, 0.9510565162951535312, 1.000000000000000000, 0.9510565162951535312, 1.000000000000000000, 0.9510565162951535312, 1.000000000000000000, 0.9510565162951535312, 1.000000000000000000, 0.9510565162951535312, 1.000000000000000000, 0.9510565162951535312, 1.000000000000000000, 0.9510565162951535312, 1.000000000000000000, 0.9510565162951535312, 1.000000000000000000, 0.9510565162951535312, 1.000000000000000000, 0.9510565162951535312, 1.000000000000000000, 0.9510565162951535312, 1.000000000000000000, 0.9510565162951535312, 1.000000000000000000, 0.9510565162951535312, 1.000000000000000000, 0.9510565162951535312, 1.000000000000000000, 0.9510565162951535312, 1.000000000000000000, 0.9510565162951535312, 1.000000000000000000, 0.9510565162951535312, 1.000000000000000000, 0.9510565162951535312, 1.000000000000000000, 0.9510565162951535312, 1.000000000000000000, 0.9510565162951535312, 1.000000000000000000, 0.9510565162951535312, 1.000000000000000000, 0.9510565162951535312, 1.000000000000000000, 0.9510565162951535312, 1.000000000000000000, 0.9510565162951535312, 1.000000000000000000, 0.9510565162951535312, 1.000000000000000000, 0.9510565162951535312, 1.000000000000000000, 0.9510565162951535312, 1.000000000000000000, 0.9510565162951535312, 1.000000000000000000, 0.9510565162951535312, 1.000000000000000000, 0.9510565162951535312, 1.000000000000000000, 0.9510565162951535312, 1.000000000000000000, 0.9510565162951535312, 1.000000000000000000, 0.9510565162951535312, 1.000000000000000000, 0.9510565162951535312, 1.000000000000000000, 0.9510565162951535312, 1.000000000000000000, 0.9510565162951535312, 1.000000000000000000, 0.9510565162951535312, 1.000000000000000000, 0.9510565162951535312, 1.000000000000000000, 0.9510565162951535312, 1.000000000000000000, 0.9510565162951535312, 1.000000000000000000, 0.9510565162951535312, 1.000000000000000000, 0.9510565162951535312, 1.000000000000000000, 0.9510565162951535312, 1.000000000000000000, 0.9510565162951535312, 1.000000000000000000, 0.9510565162951535312, 1.000000000000000000, 0.9510565162951535312, 1.000000000000000000, 0.9510565162951535312, 1.000000000000000000, 0.9510565162951535312, 1.000000000000000000, 0.9510565162951535312, 1.000000000000000000, 0.9510565162951535312, 1.000000000000000000, 0.9510565162951535312, 1.000000000000000000, 0.9510565162951535312, 1.000000000000000000, 0.9510565162951535312, 1.000000000000000000, 0.9510565162951535312, 1.000000000000000000, 0.9510565162951535312, 1.000000000000000000, 0.9510565162951535312, 1.000000000000000000, 0.9510565162951535312, 1.000000000000000000, 0.9510565162951535312, 1.000000000000000000, 0.9510565162951535312, 1.000000000000000000, 0.9510565162951535312, 1.000000000000000000, 0.9510565162951535312, 1.000000000000000000, 0.9510565162951535312, 1.000000000000000000, 0.9510565162951535312, 1.000000000000000000, 0.9510565162951535312, 1.000000000000000000, 0.9510565162951535312, 1.000000000000000000, 0.9510565162951535312, 1.000000000000000000, 0.9510565162951535312, 1.000000000000000000, 0.9510565162951535312, 1.000000000000000000, 0.9510565162951535312, 1.000000000000000000, 0.9510565162951535312, 1.000000000000000000, 0.9510565162951535312, 1.000000000000000000, 0.9510565162951535312, 1.000000000000000000, 0.9510565162951535312, 1.000000000000000000, 0.9510565162951535312, 1.000000000000000000, 0.9510565162951535312, 1.000000000000000000, 0.9510565162951535312, 1.000000000000000000, 0.9510565162951535312, 1.000000000000000000, 0.9510565162951535312, 1.000000000000000000, 0.9510565162951535312, 1.000000000000000000, 0.9510565162951535312, 1.000000000000000000, 0.9510565162951535312, 1.000000000000000000, 0.9510565162951535312, 1.000000000000000000, 0.9510565162951535312, 1.000000000000000000, 0.9510565162951535312, 1.000000000000000000, 0.9510565162951535312, 1.000000000000000000, 0.9510565162951535312, 1.000000000000000000, 0.9510565162951535312, 1.000000000000000000, 0.9510565162951535312, 1.000000000000000000, 0.9510565162951535312, 1.000000000000000000, 0.9510565162951535312, 1.000000000000000000, 0.9510565162951535312, 1.000000000000000000, 0.9510565162951535312, 1.000000000000000000, 0.9510565162951535312, 1.000000000000000000, 0.9510565162951535312, 1.000000000000000000, 0.9510565162951535312, 1.000000000000000000, 0.9510565162951535312, 1.000000000000000000, 0.9510565162951535312, 1.000000000000000000, 0.9510565162951535312, 1.000000000000000000, 0.9510565162951535312, 1.000000000000000000, 0.9510565162951535312, 1.000000000000000000, 0.9510565162951535312, 1.000000000000000000, 0.9510565162951535312, 1.000000000000000000, 0.9510565162951535312, 1.000000000000000000, 0.9510565162951535312, 1.000000000000000000, 0.9510565162951535312, 1.000000000000000000, 0.9510565162951535312, 1.000000000000000000, 0.9510565162951535312, 1.000000000000000000, 0.9510565162951535312, 1.000000000000000000, 0.9510565162951535312, 1.000000000000000000, 0.9510565162951535312, 1.000000000000000000, 0.9510565162951535312, 1.000000000000000000, 0.9510565162951535312, 1.000000000000000000, 0.9510565162951535312, 1.000000000000000000, 0.9510565162951535312, 1.000000000000000000, 0.9510565162951535312, 1.000000000000000000, 0.9510565162951535312, 1.000000000000000000, 0.9510565162951535312, 1.000000000000000000, 0.9510565162951535312, 1.000000000000000000, 0.9510565162951535312, 1.000000000000000000, 0.9510565162951535312, 1.000000000000000000, 0.9510565162951535312, 1.000000000000000000, 0.9510565162951535312, 1.000000000000000000, 0.9510565162951535312, 1.000000000000000000, 0.9510565162951535312, 1.000000000000000000, 0.9510565162951535312, 1.000000000000000000, 0.9510565162951535312, 1.000000000000000000, 0.9510565162951535312, 1.000000000000000000, 0.9510565162951535312, 1.000000000000000000, 0.9510565162951535312, 1.000000000000000000, 0.9510565162951535312, 1.000000000000000000, 0.9510565162951535312, 1.000000000000000000, 0.9510565162951535312, 1.000000000000000000, 0.9510565162951535312, 1.000000000000000000, 0.9510565162951535312, 1.000000000000000000, 0.9510565162951535312, 1.000000000000000000, 0.9510565162951535312, 1.000000000000000000, 0.9510565162951535312, 1.000000000000000000, 0.9510565162951535312, 1.000000000000000000, 0.9510565162951535312, 1.000000000000000000, 0.9510565162951535312, 1.000000000000000000, 0.9510565162951535312, 1.000000000000000000, 0.9510565162951535312, 1.000000000000000000, 0.9510565162951535312, 1.000000000000000000, 0.9510565162951535312, 1.000000000000000000, 0.9510565162951535312, 1.000000000000000000, 0.9510565162951535312, 1.000000000000000000, 0.9510565162951535312, 1.000000000000000000, 0.9510565162951535312, 1.000000000000000000, 0.9510565162951535312, 1.000000000000000000, 0.9510565162951535312, 1.000000000000000000, 0.9510565162951535312, 1.000000000000000000, 0.9510565162951535312, 1.000000000000000000, 0.9510565162951535312, 1.000000000000000000, 0.9510565162951535312, 1.000000000000000000, 0.9510565162951535312, 1.000000000000000000, 0.9510565162951535312, 1.000000000000000000, 0.9510565162951535312, 1.000000000000000000, 0.9510565162951535312, 1.000000000000000000, 0.9510565162951535312, 1.000000000000000000, 0.9510565162951535312, 1.000000000000000000, 0.9510565162951535312, 1.000000000000000000, 0.9510565162951535312, 1.000000000000000000, 0.9510565162951535312, 1.000000000000000000, 0.9510565162951535312, 1.000000000000000000, 0.9510565162951535312, 1.000000000000000000, 0.9510565162951535312, 1.000000000000000000, 0.9510565162951535312, 1.000000000000000000, 0.9510565162951535312, 1.000000000000000000, 0.9510565162951535312, 1.000000000000000000, 0.9510565162951535312, 1.000000000000000000, 0.9510565162951535312, 1.000000000000000000, 0.9510565162951535312, 1.000000000000000000, 0.9510565162951535312, 1.000000000000000000, 0.9510565162951535312, 1.000000000000000000, 0.9510565162951535312, 1.000000000000000000, 0.9510565162951535312, 1.000000000000000000, 0.9510565162951535312, 1.000000000000000000, 0.9510565162951535312, 1.000000000000000000, 0.9510565162951535312, 1.000000000000000000, 0.9510565162951535312, 1.000000000000000000, 0.9510565162951535312, 1.000000000000000000, 0.9510565162951535312, 1.000000000000000000, 0.9510565162951535312, 1.000000000000000000, 0.9510565162951535312, 1.000000000000000000, 0.9510565162951535312, 1.000000000000000000, 0.9510565162951535312, 1.000000000000000000, 0.9510565162951535312, 1.000000000000000000, 0.9510565162951535312, 1.000000000000000000, 0.9510565162951535312, 1.000000000000000000, 0.9510565162951535312, 1.000000000000000000, 0.9510565162951535312, 1.000000000000000000, 0.9510565162951535312, 1.000000000000000000, 0.9510565162951535312, 1.000000000000000000, 0.9510565162951535312, 1.000000000000000000, 0.9510565162951535312, 1.000000000000000000, 0.9510565162951535312, 1.000000000000000000, 0.9510565162951535312, 1.000000000000000000, 0.9510565162951535312, 1.000000000000000000, 0.9510565162951535312, 1.000000000000000000, 0.9510565162951535312, 1.000000000000000000, 0.9510565162951535312, 1.000000000000000000, 0.9510565162951535312, 1.000000000000000000, 0.9510565162951535312, 1.000000000000000000, 0.9510565162951535312, 1.000000000000000000, 0.9510565162951535312, 1.000000000000000000, 0.9510565162951535312, 1.000000000000000000, 0.9510565162951535312, 1.000000000000000000, 0.9510565162951535312, 1.000000000000000000, 0.9510565162951535312, 1.000000000000000000, 0.9510565162951535312, 1.000000000000000000, 0.9510565162951535312, 1.000000000000000000, 0.9510565162951535312, 1.000000000000000000, 0.9510565162951535312, 1.000000000000000000, 0.9510565162951535312, 1.000000000000000000, 0.9510565162951535312, 1.000000000000000000, 0.9510565162951535312, 1.000000000000000000, 0.9510565162951535312, 1.000000000000000000, 0.9510565162951535312, 1.000000000000000000, 0.9510565162951535312, 1.000000000000000000, 0.9510565162951535312, 1.000000000000000000, 0.9510565162951535312, 1.000000000000000000, 0.9510565162951535312, 1.000000000000000000, 0.9510565162951535312, 1.000000000000000000, 0.9510565162951535312, 1.000000000000000000, 0.9510565162951535312, 1.000000000000000000, 0.9510565162951535312, 1.000000000000000000, 0.9510565162951535312, 1.000000000000000000, 0.9836246098489007661, 0.9782068950532306628) ) ) 
 REPRESENTATION_ITEM ( '' )  SURFACE ( )  );
#11641 = CARTESIAN_POINT ( 'NONE',  ( -142.0420953463936087, -162.3938272943107393, 49.65701158161630957 ) ) ;
#11642 = CARTESIAN_POINT ( 'NONE',  ( 42.21948215057684450, 155.1113394311928460, 29.21067981925357060 ) ) ;
#11643 = CARTESIAN_POINT ( 'NONE',  ( -141.4692556286852891, -177.2130981290892748, 52.90620854394536821 ) ) ;
#11644 = CARTESIAN_POINT ( 'NONE',  ( 46.10157429594899270, 151.7344580088725934, 29.95742577749337343 ) ) ;
#11645 = CARTESIAN_POINT ( 'NONE',  ( 41.64333658814960870, 120.9797705074273182, 38.42115945441014446 ) ) ;
#11646 = CARTESIAN_POINT ( 'NONE',  ( 75.17075062522994244, 131.8760474256973509, 11.19198414525841301 ) ) ;
#11647 = CARTESIAN_POINT ( 'NONE',  ( 38.96631938032478359, 115.0104996726487485, 37.14960608071593384 ) ) ;
#11648 = CARTESIAN_POINT ( 'NONE',  ( 39.42975644700377558, 120.4151871740940010, 36.81289934271958941 ) ) ;
#11649 = LINE ( 'NONE', #11316, #10432 ) ;
#11650 = CARTESIAN_POINT ( 'NONE',  ( 14.82542406694137860, 100.6198891296320994, 2.415082931867933880 ) ) ;
#11651 = CARTESIAN_POINT ( 'NONE',  ( 38.24087231542673493, 147.7000375650850970, 3.727681574521009900 ) ) ;
#11652 = CARTESIAN_POINT ( 'NONE',  ( 45.22504609509771001, 59.11591859955431971, 30.37668211462113277 ) ) ;
#11653 = CARTESIAN_POINT ( 'NONE',  ( 38.58424406990785371, 96.52977050742731535, 35.64915139335015937 ) ) ;
#11654 = ORIENTED_EDGE ( 'NONE', *, *, #8140, .F. ) ;
#11655 = DIRECTION ( 'NONE',  ( 0.000000000000000000, 1.000000000000000000, 0.000000000000000000 ) ) ;
#11656 = ORIENTED_EDGE ( 'NONE', *, *, #11810, .T. ) ;
#11657 = CARTESIAN_POINT ( 'NONE',  ( 48.01140435219951996, 85.43445800887255359, 32.58608133808903773 ) ) ;
#11658 = DIRECTION ( 'NONE',  ( 0.000000000000000000, 0.000000000000000000, 1.000000000000000000 ) ) ;
#11659 = CARTESIAN_POINT ( 'NONE',  ( 48.01140435219951996, 143.3604996726487570, 32.58608133808903773 ) ) ;
#11661 = CARTESIAN_POINT ( 'NONE',  ( 69.71546013739904879, 111.0973159356150717, 7.018072855358342466 ) ) ;
#11660 = CARTESIAN_POINT ( 'NONE',  ( 39.42975644700377558, 99.41518717409400097, 36.81289934271958941 ) ) ;
#11662 = CARTESIAN_POINT ( 'NONE',  ( -142.0420953463936087, -171.6584106276440593, 49.65701158161630957 ) ) ;
#11663 = CARTESIAN_POINT ( 'NONE',  ( -159.0959885057557983, -194.1938272943107222, 44.11586579668791330 ) ) ;
#11665 = CYLINDRICAL_SURFACE ( 'NONE', #11842, 10.00000000000000888 ) ;
#11664 = CARTESIAN_POINT ( 'NONE',  ( 116.4417310231185780, -126.9891397928655010, 30.00000000000000000 ) ) ;
#11666 = DIRECTION ( 'NONE',  ( -0.5061580162706792452, -0.8624407588727071028, 0.000000000000000000 ) ) ;
#11667 = VECTOR ( 'NONE', #5238, 1000.000000000000114 ) ;
#11668 = APPLICATION_CONTEXT ( 'automotive_design' ) ;
#11669 = AXIS2_PLACEMENT_3D ( 'NONE', #1901, #7311, #14012 ) ;
#11670 = CARTESIAN_POINT ( 'NONE',  ( 43.01140435219951286, 146.9604996726487229, 29.21067981925356705 ) ) ;
#11671 = CARTESIAN_POINT ( 'NONE',  ( 41.46631938032478359, 78.11049967264874283, 29.45539723777780239 ) ) ;
#11672 = CARTESIAN_POINT ( 'NONE',  ( 46.59305225739526435, 149.1797705074273210, 31.60846029578754468 ) ) ;
#11673 = CARTESIAN_POINT ( 'NONE',  ( 42.21948215057684450, 63.45757658655229250, 39.21067981925355639 ) ) ;
#11674 = CARTESIAN_POINT ( 'NONE',  ( 26.13368487350976110, 90.12329638092472806, 0.9106621812756837686 ) ) ;
#11675 = CARTESIAN_POINT ( 'NONE',  ( 43.01140435219951286, 141.8651871740940180, 38.86567161673127657 ) ) ;
#11676 = CIRCLE ( 'NONE', #6409, 576.1986910693910886 ) ;
#11677 = CARTESIAN_POINT ( 'NONE',  ( -148.5561028927606344, -161.7938272943107449, 40.69124936498395328 ) ) ;
#11678 = CARTESIAN_POINT ( 'NONE',  ( -157.2955611005345986, -173.6084106276440480, 41.63779006702063867 ) ) ;
#11679 = VERTEX_POINT ( 'NONE', #18916 ) ;
#11680 = CARTESIAN_POINT ( 'NONE',  ( 162.3411339277076308, 184.7625696037766261, -5.999999999999976019 ) ) ;
#11681 = CARTESIAN_POINT ( 'NONE',  ( -154.3824083646099439, -158.7584106276440536, 40.69124936498395328 ) ) ;
#11682 = CARTESIAN_POINT ( 'NONE',  ( 37.44377528459369131, 147.6348322250013894, 2.699600794211013621 ) ) ;
#11683 = CARTESIAN_POINT ( 'NONE',  ( 41.46631938032478359, 134.1844580088725820, 29.45539723777780239 ) ) ;
#11684 = CARTESIAN_POINT ( 'NONE',  ( 47.43856463449118621, 121.6151871740940038, 34.21067981925357060 ) ) ;
#11685 = ORIENTED_EDGE ( 'NONE', *, *, #4149, .F. ) ;
#11686 = EDGE_LOOP ( 'NONE', ( #13129, #113, #18897, #9365 ) ) ;
#11687 = VECTOR ( 'NONE', #15033, 1000.000000000000000 ) ;
#11688 = CARTESIAN_POINT ( 'NONE',  ( 38.01140435219952707, 146.7844580088725763, 34.21067981925357060 ) ) ;
#11689 = ORIENTED_EDGE ( 'NONE', *, *, #10773, .T. ) ;
#11690 = CARTESIAN_POINT ( 'NONE',  ( 38.01140435219951996, 110.9344580088725678, 35.83527830041810347 ) ) ;
#11691 = CARTESIAN_POINT ( 'NONE',  ( 47.43856463449118621, 154.8797705074273097, 34.21067981925357060 ) ) ;
#11692 = CARTESIAN_POINT ( 'NONE',  ( 47.43856463449118621, 70.87977050742732388, 34.21067981925357060 ) ) ;
#11694 = CARTESIAN_POINT ( 'NONE',  ( 65.09246388851926213, 137.4469437283422906, 4.918530982704383270 ) ) ;
#11693 = CARTESIAN_POINT ( 'NONE',  ( 45.74753988029933538, 128.0651871740940067, 30.44471234641811819 ) ) ;
#11695 = CARTESIAN_POINT ( 'NONE',  ( 46.10157429594899270, 86.66049967264872578, 29.95742577749337343 ) ) ;
#11696 = CARTESIAN_POINT ( 'NONE',  ( 26.66797635711824199, 149.9459070286683868, 17.30505193804556185 ) ) ;
#11697 = CARTESIAN_POINT ( 'NONE',  ( -143.3790856849358306, -170.7630981290892862, 43.77915905869157598 ) ) ;
#11698 = DIRECTION ( 'NONE',  ( -0.8510798296367590998, -0.5250363069212118372, 0.000000000000000000 ) ) ;
#11699 = CARTESIAN_POINT ( 'NONE',  ( 44.37947211624943833, 91.01518717409399528, 38.42115945441014446 ) ) ;
#11700 = CARTESIAN_POINT ( 'NONE',  ( 38.17211394134016444, 144.4343190729016442, 35.51056251760059723 ) ) ;
#11701 = LINE ( 'NONE', #15121, #7469 ) ;
#11702 = VERTEX_POINT ( 'NONE', #1840 ) ;
#11703 = CARTESIAN_POINT ( 'NONE',  ( 44.37947211624943833, 61.27977050742732246, 38.42115945441014446 ) ) ;
#11704 = CARTESIAN_POINT ( 'NONE',  ( -145.6429501568359797, -189.2084106276440423, 41.63779006702063867 ) ) ;
#11705 = CARTESIAN_POINT ( 'NONE',  ( 20.69791174355615837, 145.8831102580302570, -4.951040100860263138 ) ) ;
#11706 = EDGE_CURVE ( 'NONE', #1555, #17127, #15286, .T. ) ;
#11707 = CARTESIAN_POINT ( 'NONE',  ( -145.6429501568359797, -178.1084106276440480, 57.67623309621198047 ) ) ;
#11708 = ORIENTED_EDGE ( 'NONE', *, *, #9214, .F. ) ;
#11709 = CARTESIAN_POINT ( 'NONE',  ( 47.43856463449117200, 154.7651871740940237, 32.77220824515698183 ) ) ;
#11710 = LINE ( 'NONE', #18102, #3233 ) ;
#11711 =( BOUNDED_CURVE ( )  B_SPLINE_CURVE ( 1, ( #21668, #18006 ),
 .UNSPECIFIED., .F., .F. ) 
 B_SPLINE_CURVE_WITH_KNOTS ( ( 2, 2 ),
 ( 0.000000000000000000, 1.000000000000000000 ),
 .UNSPECIFIED. ) 
 CURVE ( )  GEOMETRIC_REPRESENTATION_ITEM ( )  RATIONAL_B_SPLINE_CURVE ( ( 0.9782066976764483002, 0.9782066976764483002 ) ) 
 REPRESENTATION_ITEM ( '' )  );
#11712 = CARTESIAN_POINT ( 'NONE',  ( 39.42975644700377558, 111.6797705074273210, 36.81289934271958941 ) ) ;
#11713 = CARTESIAN_POINT ( 'NONE',  ( 18.86674891209848326, 143.9013856721611546, -11.04182128657428485 ) ) ;
#11714 = ORIENTED_EDGE ( 'NONE', *, *, #6385, .F. ) ;
#11715 = CARTESIAN_POINT ( 'NONE',  ( 29.22050282933603071, 144.5044581412665536, -3.652897588741476742 ) ) ;
#11716 = ORIENTED_EDGE ( 'NONE', *, *, #20429, .F. ) ;
#11717 = CARTESIAN_POINT ( 'NONE',  ( 40.27526882409969033, 117.8297705074273267, 37.97664729208901946 ) ) ;
#11718 = CARTESIAN_POINT ( 'NONE',  ( -39.63192160874127978, -37.13255853780189852, -35.00000000000000000 ) ) ;
#11719 = CARTESIAN_POINT ( 'NONE',  ( 45.74753988029933538, 157.1651871740940010, 37.97664729208901946 ) ) ;
#11720 = CARTESIAN_POINT ( 'NONE',  ( 77.15313604554262383, 122.4041478163663612, -8.494263314424808087 ) ) ;
#11721 = CARTESIAN_POINT ( 'NONE',  ( 38.01140435219952707, 107.6344580088725706, 32.58608133808903773 ) ) ;
#11722 = LINE ( 'NONE', #10303, #11338 ) ;
#11723 = CYLINDRICAL_SURFACE ( 'NONE', #13173, 10.00000000000000888 ) ;
#11724 = CARTESIAN_POINT ( 'NONE',  ( -151.4692556286852891, -175.7391397928654442, 60.17163382399899518 ) ) ;
#11725 = CARTESIAN_POINT ( 'NONE',  ( 42.21948215057684450, 157.3836182503284533, 39.21067981925355639 ) ) ;
#11726 = DIRECTION ( 'NONE',  ( -0.000000000000000000, -0.000000000000000000, -1.000000000000000000 ) ) ;
#11727 = DIRECTION ( 'NONE',  ( -0.000000000000000000, 0.000000000000000000, -1.000000000000000000 ) ) ;
#11728 = APPLICATION_PROTOCOL_DEFINITION ( 'draft international standard', 'automotive_design', 1998, #19855 ) ;
#11729 = CARTESIAN_POINT ( 'NONE',  ( -124.3720331620955619, 13.78046159333444720, 4.000000000000021316 ) ) ;
#11730 = CARTESIAN_POINT ( 'NONE',  ( 46.59305225739526435, 91.57977050742731251, 36.81289934271958941 ) ) ;
#11731 = CARTESIAN_POINT ( 'NONE',  ( 67.98812442775457043, 106.8157236907426153, -0.7957547315468347371 ) ) ;
#11732 = CARTESIAN_POINT ( 'NONE',  ( -148.5561028927606344, -177.9938272943107336, 58.62277379824867296 ) ) ;
#11733 = CARTESIAN_POINT ( 'NONE',  ( 44.37947211624943833, 91.01518717409399528, 38.42115945441014446 ) ) ;
#11734 = CARTESIAN_POINT ( 'NONE',  ( 0.000000000000000000, -136.9891397928655010, 30.00000000000000000 ) ) ;
#11735 = ORIENTED_EDGE ( 'NONE', *, *, #4729, .T. ) ;
#11736 = CARTESIAN_POINT ( 'NONE',  ( -141.4692556286852891, -190.1391397928654783, 52.90620854394536821 ) ) ;
#11737 = CARTESIAN_POINT ( 'NONE',  ( 75.59501567365037999, 109.4093883240155378, 12.93430809701916750 ) ) ;
#11738 = CARTESIAN_POINT ( 'NONE',  ( 45.74753988029934249, 143.3297705074272983, 30.44471234641812174 ) ) ;
#11739 = CARTESIAN_POINT ( 'NONE',  ( 51.61786746416480298, 93.13668562621728597, 1.065498654441493720 ) ) ;
#11740 = EDGE_CURVE ( 'NONE', #7746, #2272, #12481, .T. ) ;
#11741 = CARTESIAN_POINT ( 'NONE',  ( 45.74753988029934249, 61.42977050742731393, 37.97664729208901235 ) ) ;
#11742 = EDGE_LOOP ( 'NONE', ( #14253, #15894, #11685, #2678 ) ) ;
#11743 = CARTESIAN_POINT ( 'NONE',  ( 41.64333658814960870, 143.7797705074273154, 30.00020018409699318 ) ) ;
#11744 = CARTESIAN_POINT ( 'NONE',  ( 47.43856463449117200, 95.02977050742730114, 32.77220824515698183 ) ) ;
#11745 = CARTESIAN_POINT ( 'NONE',  ( 184.5838786899744832, 207.5897843508632263, 23.27362312593913174 ) ) ;
#11746 = CARTESIAN_POINT ( 'NONE',  ( 38.96631938032478359, 105.4104996726487400, 31.27175355779120025 ) ) ;
#11747 = CARTESIAN_POINT ( 'NONE',  ( 43.01140435219951286, 59.36518717409399670, 29.55568802177586463 ) ) ;
#11748 = CARTESIAN_POINT ( 'NONE',  ( 72.34521997529867576, 314.8592298662555322, 4.000000000000003553 ) ) ;
#11749 = CARTESIAN_POINT ( 'NONE',  ( -145.6429501568359797, -161.9438272943107222, 41.63779006702063867 ) ) ;
#11750 = CARTESIAN_POINT ( 'NONE',  ( 163.1026836591718734, 192.4288937294299160, 14.00000000000001776 ) ) ;
#11751 = CARTESIAN_POINT ( 'NONE',  ( -157.6495955161842062, -172.1130981290892805, 58.16351966513671812 ) ) ;
#11752 = CARTESIAN_POINT ( 'NONE',  ( 38.96631938032478359, 112.0104996726487485, 37.14960608071593384 ) ) ;
#11753 = EDGE_CURVE ( 'NONE', #4439, #3828, #18594, .T. ) ;
#11754 = CARTESIAN_POINT ( 'NONE',  ( 41.46631938032478359, 141.3844580088725991, 38.96596240072933170 ) ) ;
#11755 = CARTESIAN_POINT ( 'NONE',  ( 47.43856463449117200, 125.0297705074273011, 32.77220824515698183 ) ) ;
#11756 = CARTESIAN_POINT ( 'NONE',  ( 51.59368247783319816, 153.1301807948854616, 10.12058642595840929 ) ) ;
#11757 = DIRECTION ( 'NONE',  ( 0.3450121214752274179, -0.9385982292947088190, 0.000000000000000000 ) ) ;
#11758 = CARTESIAN_POINT ( 'NONE',  ( 46.59305225739526435, 118.3151871740940067, 36.81289934271958941 ) ) ;
#11759 = CARTESIAN_POINT ( 'NONE',  ( -153.0531000319306827, -183.1622583705452314, 39.65701158161630957 ) ) ;
#11760 = DIRECTION ( 'NONE',  ( 0.5010362705417047424, 0.000000000000000000, 0.8654262854811261008 ) ) ;
#11761 = CARTESIAN_POINT ( 'NONE',  ( 75.45202302719175691, 109.2280190411066059, 6.938704244663667531 ) ) ;
#11762 = ADVANCED_FACE ( 'NONE', ( #21115 ), #724, .F. ) ;
#11763 = CARTESIAN_POINT ( 'NONE',  ( 44.18632541912793243, 91.73153706005567187, -6.629209314582290347 ) ) ;
#11764 = CARTESIAN_POINT ( 'NONE',  ( -143.3790856849358306, -155.7630981290893146, 43.77915905869157598 ) ) ;
#11765 = CARTESIAN_POINT ( 'NONE',  ( 39.42975644700377558, 84.07977050742732672, 31.60846029578754468 ) ) ;
#11766 = AXIS2_PLACEMENT_3D ( 'NONE', #6188, #10945, #9405 ) ;
#11767 = ORIENTED_EDGE ( 'NONE', *, *, #11107, .T. ) ;
#11768 = EDGE_CURVE ( 'NONE', #21314, #5667, #20786, .T. ) ;
#11769 = CARTESIAN_POINT ( 'NONE',  ( -141.4692556286852891, -168.0630981290893260, 49.65701158161630957 ) ) ;
#11770 = EDGE_LOOP ( 'NONE', ( #15079, #21540, #14501, #21735 ) ) ;
#11771 =( BOUNDED_CURVE ( )  B_SPLINE_CURVE ( 2, ( #8096, #19773, #1040, #12941, #11276 ),
 .UNSPECIFIED., .F., .T. ) 
 B_SPLINE_CURVE_WITH_KNOTS ( ( 3, 2, 3 ),
 ( 0.9464285714285713969, 0.9499999999999999556, 0.9523897199067097308 ),
 .UNSPECIFIED. ) 
 CURVE ( )  GEOMETRIC_REPRESENTATION_ITEM ( )  RATIONAL_B_SPLINE_CURVE ( ( 0.9755282581475768211, 0.9755282581475768211, 1.000000000000000000, 0.9836254295761526212, 0.9782074374858980015 ) ) 
 REPRESENTATION_ITEM ( '' )  );
#11772 = CARTESIAN_POINT ( 'NONE',  ( 38.01140435219951996, 74.93445800887258201, 35.83527830041810347 ) ) ;
#11773 = CARTESIAN_POINT ( 'NONE',  ( 41.46631938032478359, 60.38445800887257064, 38.96596240072933170 ) ) ;
#11774 = CARTESIAN_POINT ( 'NONE',  ( 38.96631938032478359, 139.0104996726487627, 37.14960608071593384 ) ) ;
#11776 = CARTESIAN_POINT ( 'NONE',  ( 71.58903643207423784, 138.6103067756119742, -8.061014907923841122 ) ) ;
#11775 = CARTESIAN_POINT ( 'NONE',  ( 43.01140435219951286, 87.86518717409397539, 38.86567161673127657 ) ) ;
#11777 = CARTESIAN_POINT ( 'NONE',  ( -159.0959885057557983, -161.4584106276440423, 44.11586579668791330 ) ) ;
#11778 = CARTESIAN_POINT ( 'NONE',  ( -142.0420953463935803, -192.2438272943107336, 46.59394152635518083 ) ) ;
#11779 = CARTESIAN_POINT ( 'NONE',  ( -81.61981105773979550, 604.5992151483073940, -0.8325491102011938205 ) ) ;
#11780 = CARTESIAN_POINT ( 'NONE',  ( 161.4773229304660731, 84.89323405393692212, 14.00000000000001776 ) ) ;
#11781 = EDGE_CURVE ( 'NONE', #5965, #7305, #16272, .T. ) ;
#11782 = CARTESIAN_POINT ( 'NONE',  ( -149.8854112254399524, -177.7362167067690564, 59.65701158161632378 ) ) ;
#11783 = CARTESIAN_POINT ( 'NONE',  ( 46.10157429594899270, 145.7604996726487627, 38.46393386101375711 ) ) ;
#11784 = CARTESIAN_POINT ( 'NONE',  ( 46.59305225739526435, 155.1797705074273210, 31.60846029578754468 ) ) ;
#11785 = DIRECTION ( 'NONE',  ( 0.5000000000000002220, 0.000000000000000000, -0.8660254037844384856 ) ) ;
#11786 = CARTESIAN_POINT ( 'NONE',  ( 9.656473946750173454, 127.6128973189080398, 2.339233609801092406 ) ) ;
#11787 = CARTESIAN_POINT ( 'NONE',  ( 44.37947211624943833, 146.2151871740940123, 30.00020018409699318 ) ) ;
#11788 = CARTESIAN_POINT ( 'NONE',  ( -154.3824083646099439, -163.2938272943107449, 58.62277379824867296 ) ) ;
#11789 = CARTESIAN_POINT ( 'NONE',  ( -142.0420953463935803, -171.8084106276440082, 52.72008163687743831 ) ) ;
#11790 = EDGE_CURVE ( 'NONE', #4098, #11964, #20099, .T. ) ;
#11791 = EDGE_LOOP ( 'NONE', ( #16443, #5697 ) ) ;
#11792 = LINE ( 'NONE', #114, #20140 ) ;
#11793 = CARTESIAN_POINT ( 'NONE',  ( -145.6429501568359797, -157.1084106276440480, 57.67623309621198047 ) ) ;
#11794 = CARTESIAN_POINT ( 'NONE',  ( 26.48090744323847190, 142.7828511622217889, -4.776412194962503577 ) ) ;
#11795 = CARTESIAN_POINT ( 'NONE',  ( 43.01140435219951286, 134.0344580088725763, 29.21067981925356705 ) ) ;
#11796 = CARTESIAN_POINT ( 'NONE',  ( 45.74753988029933538, 124.1651871740940152, 37.97664729208901946 ) ) ;
#11797 = VERTEX_POINT ( 'NONE', #11179 ) ;
#11798 = ORIENTED_EDGE ( 'NONE', *, *, #13500, .F. ) ;
#11799 = CARTESIAN_POINT ( 'NONE',  ( -153.0531000319306827, -161.2362167067690280, 39.65701158161629536 ) ) ;
#11800 = ORIENTED_EDGE ( 'NONE', *, *, #1784, .T. ) ;
#11801 = CARTESIAN_POINT ( 'NONE',  ( 38.01140435219951996, 98.63445800887255643, 32.58608133808903773 ) ) ;
#11802 = CARTESIAN_POINT ( 'NONE',  ( 41.64333658814960870, 158.7797705074273438, 30.00020018409699318 ) ) ;
#11803 = CARTESIAN_POINT ( 'NONE',  ( 38.58424406990786082, 69.37977050742730967, 34.21067981925357060 ) ) ;
#11805 = CARTESIAN_POINT ( 'NONE',  ( 41.83412315030695794, 148.0818998446914634, 10.87053871734362431 ) ) ;
#11804 = CARTESIAN_POINT ( 'NONE',  ( 43.01140435219951286, 128.3651871740940180, 29.55568802177586463 ) ) ;
#11806 = CARTESIAN_POINT ( 'NONE',  ( 43.01140435219951286, 80.96049967264872294, 28.95336869806222779 ) ) ;
#11807 = FACE_OUTER_BOUND ( 'NONE', #16859, .T. ) ;
#11808 = AXIS2_PLACEMENT_3D ( 'NONE', #18274, #9803, #19597 ) ;
#11809 = EDGE_CURVE ( 'NONE', #14927, #13022, #14729, .T. ) ;
#11810 = EDGE_CURVE ( 'NONE', #17093, #1013, #20894, .T. ) ;
#11811 = CARTESIAN_POINT ( 'NONE',  ( 141.1725454929228079, -61.68114226949890622, 19.99999999999998934 ) ) ;
#11812 = CARTESIAN_POINT ( 'NONE',  ( 43.01140435219950575, 139.4604996726487514, 39.21067981925356349 ) ) ;
#11813 = CARTESIAN_POINT ( 'NONE',  ( 47.43856463449117200, 82.46518717409398391, 35.64915139335016647 ) ) ;
#11814 = CARTESIAN_POINT ( 'NONE',  ( 39.70855384287648349, 144.6890526212906991, 30.44250125826515685 ) ) ;
#11815 = DIRECTION ( 'NONE',  ( -0.7071067811865456854, 8.659560562354910671E-17, 0.7071067811865493491 ) ) ;
#11816 = ORIENTED_EDGE ( 'NONE', *, *, #3276, .F. ) ;
#11817 = CARTESIAN_POINT ( 'NONE',  ( 43.01140435219951286, 61.12977050742731677, 38.86567161673127657 ) ) ;
#11818 = CARTESIAN_POINT ( 'NONE',  ( -142.0420953463935803, -186.5084106276440536, 46.59394152635518793 ) ) ;
#11819 = CARTESIAN_POINT ( 'NONE',  ( 18.65831473100296023, 143.8050973582651579, -5.046215916575388150 ) ) ;
#11820 = CARTESIAN_POINT ( 'NONE',  ( -143.8425227516148084, -174.3584106276440480, 44.11586579668791330 ) ) ;
#11821 = ORIENTED_EDGE ( 'NONE', *, *, #16085, .T. ) ;
#11822 = CARTESIAN_POINT ( 'NONE',  ( 38.58424406990784661, 150.2651871740940237, 35.64915139335016647 ) ) ;
#11823 = LINE ( 'NONE', #14797, #2173 ) ;
#11824 = CARTESIAN_POINT ( 'NONE',  ( 44.37947211624943833, 115.2797705074273296, 38.42115945441014446 ) ) ;
#11825 = CARTESIAN_POINT ( 'NONE',  ( 73.72238702602700755, 135.0318370961144296, 5.077453337991364002 ) ) ;
#11826 = ORIENTED_EDGE ( 'NONE', *, *, #4067, .T. ) ;
#11827 = AXIS2_PLACEMENT_3D ( 'NONE', #19754, #18318, #11472 ) ;
#11828 = CARTESIAN_POINT ( 'NONE',  ( 62.66823040046688931, 140.1266048904901993, -2.224326160187301227 ) ) ;
#11829 = ORIENTED_EDGE ( 'NONE', *, *, #17001, .T. ) ;
#11830 = CARTESIAN_POINT ( 'NONE',  ( 45.74753988029933538, 118.4297705074272926, 37.97664729208901946 ) ) ;
#11831 = CARTESIAN_POINT ( 'NONE',  ( 42.21948215057684450, 126.0373810949690210, 29.21067981925356705 ) ) ;
#11832 = CARTESIAN_POINT ( 'NONE',  ( 45.74753988029933538, 86.32977050742729830, 30.44471234641811819 ) ) ;
#11833 = CARTESIAN_POINT ( 'NONE',  ( 40.27526882409969033, 155.6651871740940010, 30.44471234641811819 ) ) ;
#11834 = EDGE_CURVE ( 'NONE', #15585, #11274, #14262, .T. ) ;
#11835 = CARTESIAN_POINT ( 'NONE',  ( 70.33053884415087964, 140.4045759698336724, 5.867304552604015733 ) ) ;
#11836 = CARTESIAN_POINT ( 'NONE',  ( 54.85617982533818804, 239.2521282348021714, -19.99999999999996092 ) ) ;
#11837 = DIRECTION ( 'NONE',  ( 0.000000000000000000, 0.000000000000000000, 1.000000000000000000 ) ) ;
#11838 = CARTESIAN_POINT ( 'NONE',  ( -151.4692556286852891, -181.7391397928654726, 60.17163382399899518 ) ) ;
#11839 = CARTESIAN_POINT ( 'NONE',  ( -161.4692556286852891, -181.7130981290893033, 46.40781461928724383 ) ) ;
#11840 = CARTESIAN_POINT ( 'NONE',  ( -161.4692556286853176, -194.4891397928654726, 49.65701158161630957 ) ) ;
#11841 = CARTESIAN_POINT ( 'NONE',  ( 46.10157429594899270, 97.73445800887256496, 29.95742577749336988 ) ) ;
#11842 = AXIS2_PLACEMENT_3D ( 'NONE', #18403, #5066, #18289 ) ;
#11843 = CIRCLE ( 'NONE', #7279, 10.00000000000000888 ) ;
#11844 = CARTESIAN_POINT ( 'NONE',  ( 46.59305225739526435, 98.17977050742732104, 31.60846029578754468 ) ) ;
#11845 = CARTESIAN_POINT ( 'NONE',  ( 65.02675087932300357, 102.2843278501921418, -7.581721168364237151 ) ) ;
#11846 = CARTESIAN_POINT ( 'NONE',  ( -143.8425227516148084, -174.6938272943107506, 55.19815736654470584 ) ) ;
#11847 = EDGE_CURVE ( 'NONE', #460, #13715, #5900, .T. ) ;
#11848 = CARTESIAN_POINT ( 'NONE',  ( 41.64333658814960870, 86.51518717409399528, 30.00020018409699318 ) ) ;
#11849 = CARTESIAN_POINT ( 'NONE',  ( -143.3790856849358306, -195.6891397928654897, 43.77915905869157598 ) ) ;
#11850 = EDGE_LOOP ( 'NONE', ( #17237, #5349, #3753, #9045 ) ) ;
#11851 = CARTESIAN_POINT ( 'NONE',  ( 147.5268905834513475, 193.0332408774651185, -5.999999999999950262 ) ) ;
#11852 = CARTESIAN_POINT ( 'NONE',  ( 62.34613790317991544, 148.1570561279473850, 11.50573666851796339 ) ) ;
#11853 = CARTESIAN_POINT ( 'NONE',  ( 59.61500273516548276, 97.21183980732109831, 0.7083854377657419210 ) ) ;
#11854 = CARTESIAN_POINT ( 'NONE',  ( 38.96631938032478359, 120.0844580088725735, 37.14960608071593384 ) ) ;
#11855 = ORIENTED_EDGE ( 'NONE', *, *, #2604, .F. ) ;
#11856 = AXIS2_PLACEMENT_3D ( 'NONE', #7162, #17275, #10680 ) ;
#11857 = CARTESIAN_POINT ( 'NONE',  ( 45.74753988029933538, 149.3297705074273267, 30.44471234641811819 ) ) ;
#11858 = CARTESIAN_POINT ( 'NONE',  ( 40.27526882409969033, 98.92977050742732104, 30.44471234641811819 ) ) ;
#11859 = CIRCLE ( 'NONE', #19959, 44.28464465043163756 ) ;
#11860 = CARTESIAN_POINT ( 'NONE',  ( 43.80332655382219542, 152.8836182503285102, 29.21067981925356705 ) ) ;
#11861 = DIRECTION ( 'NONE',  ( -0.000000000000000000, 1.000000000000000000, -0.000000000000000000 ) ) ;
#11862 = CYLINDRICAL_SURFACE ( 'NONE', #18009, 10.00000000000000888 ) ;
#11863 = CARTESIAN_POINT ( 'NONE',  ( 38.01140435219952707, 153.7104996726487514, 34.21067981925357060 ) ) ;
#11864 = CARTESIAN_POINT ( 'NONE',  ( 41.46631938032478359, 109.3104996726487457, 38.96596240072933170 ) ) ;
#11865 = CARTESIAN_POINT ( 'NONE',  ( -161.4692556286852607, -169.7130981290892748, 46.40781461928724383 ) ) ;
#11866 = SHAPE_REPRESENTATION_RELATIONSHIP ( 'NONE' , 'NONE' ,  #1720, #20586 ) ;
#11867 = CARTESIAN_POINT ( 'NONE',  ( 47.05648932407426344, 145.5844580088725877, 31.27175355779120025 ) ) ;
#11868 = CARTESIAN_POINT ( 'NONE',  ( 38.58424406990784661, 126.2297705074273040, 32.77220824515698183 ) ) ;
#11869 = CARTESIAN_POINT ( 'NONE',  ( 8.737656864016759783, 121.5850998216562431, 22.14420391595633220 ) ) ;
#11870 = CARTESIAN_POINT ( 'NONE',  ( -145.2889157411863437, -183.5391397928654840, 41.15050349809589392 ) ) ;
#11871 = AXIS2_PLACEMENT_3D ( 'NONE', #17728, #6053, #5943 ) ;
#11872 = CARTESIAN_POINT ( 'NONE',  ( 41.64333658814960870, 120.7151871740939981, 38.42115945441014446 ) ) ;
#11873 = CARTESIAN_POINT ( 'NONE',  ( 126.8576204525573274, -126.9891397928655010, 67.64809332337412684 ) ) ;
#11874 = CARTESIAN_POINT ( 'NONE',  ( 75.66441332552922461, 109.8968089748874064, -0.08503035249486777525 ) ) ;
#11875 = CARTESIAN_POINT ( 'NONE',  ( 20.57499262110235350, 102.8243204193801432, -5.557751863727047770 ) ) ;
#11876 = CARTESIAN_POINT ( 'NONE',  ( -141.4692556286852891, -156.0630981290892976, 49.65701158161630957 ) ) ;
#11877 = CARTESIAN_POINT ( 'NONE',  ( 47.43856463449117911, 89.02977050742731535, 32.77220824515697473 ) ) ;
#11878 = EDGE_CURVE ( 'NONE', #6509, #8092, #640, .T. ) ;
#11879 = VERTEX_POINT ( 'NONE', #4902 ) ;
#11880 = AXIS2_PLACEMENT_3D ( 'NONE', #1023, #19648, #7759 ) ;
#11881 = CARTESIAN_POINT ( 'NONE',  ( -148.3790856849358306, -168.6630981290892919, 59.16757674456786020 ) ) ;
#11882 = CARTESIAN_POINT ( 'NONE',  ( 46.10157429594899270, 69.83445800887255928, 38.46393386101376421 ) ) ;
#11883 = CARTESIAN_POINT ( 'NONE',  ( -158.9748091281504401, -116.9891397928655010, 62.65701158161630957 ) ) ;
#11884 = CIRCLE ( 'NONE', #2046, 7.500000000000007105 ) ;
#11885 = CARTESIAN_POINT ( 'NONE',  ( 39.92123440845004723, 127.1604996726487542, 38.46393386101376421 ) ) ;
#11887 = CARTESIAN_POINT ( 'NONE',  ( 40.51949181395973199, 85.84442682937354618, -12.58519764931165241 ) ) ;
#11886 = CARTESIAN_POINT ( 'NONE',  ( 45.74753988029933538, 85.16518717409400097, 37.97664729208901946 ) ) ;
#11888 = CARTESIAN_POINT ( 'NONE',  ( -157.2955611005346270, -161.6084106276440480, 41.63779006702063867 ) ) ;
#11889 = CARTESIAN_POINT ( 'NONE',  ( -148.5561028927606344, -189.9938272943107336, 58.62277379824867296 ) ) ;
#11890 = CARTESIAN_POINT ( 'NONE',  ( 43.01140435219951286, 117.5344580088725763, 39.21067981925356349 ) ) ;
#11891 = CARTESIAN_POINT ( 'NONE',  ( 43.01140435219951286, 105.5344580088725621, 39.21067981925356349 ) ) ;
#11892 = CARTESIAN_POINT ( 'NONE',  ( 43.01140435219951286, 67.46049967264873715, 39.21067981925356349 ) ) ;
#11893 = CARTESIAN_POINT ( 'NONE',  ( -151.4692556286853176, -174.2391397928654726, 39.65701158161629536 ) ) ;
#11894 = CARTESIAN_POINT ( 'NONE',  ( 47.43856463449118621, 151.8797705074273097, 34.21067981925357060 ) ) ;
#11895 = CARTESIAN_POINT ( 'NONE',  ( -161.4692556286852891, -184.7130981290893033, 46.40781461928724383 ) ) ;
#11896 = CARTESIAN_POINT ( 'NONE',  ( 12.43312601512511151, 135.2277911470865490, 16.60371454366222466 ) ) ;
#11897 = CARTESIAN_POINT ( 'NONE',  ( 46.59305225739526435, 142.9151871740940294, 31.60846029578754468 ) ) ;
#11898 = VECTOR ( 'NONE', #10339, 1000.000000000000000 ) ;
#11899 = CARTESIAN_POINT ( 'NONE',  ( -145.6429501568359797, -164.9438272943106938, 41.63779006702063867 ) ) ;
#11900 = CARTESIAN_POINT ( 'NONE',  ( -159.0959885057557983, -172.8584106276440764, 55.19815736654470584 ) ) ;
#11901 = CARTESIAN_POINT ( 'NONE',  ( 38.58424406990785371, 62.96518717409399812, 32.77220824515697473 ) ) ;
#11902 = CARTESIAN_POINT ( 'NONE',  ( -148.5561028927606344, -162.0584106276440366, 40.69124936498395328 ) ) ;
#11903 = CARTESIAN_POINT ( 'NONE',  ( 20.05807715703862470, 136.4285572017038248, 1.866423417236719118 ) ) ;
#11904 = CARTESIAN_POINT ( 'NONE',  ( 43.01140435219951286, 123.5344580088725621, 39.21067981925356349 ) ) ;
#11905 = CARTESIAN_POINT ( 'NONE',  ( 46.59305225739526435, 127.9151871740940010, 31.60846029578754468 ) ) ;
#11906 =( BOUNDED_CURVE ( )  B_SPLINE_CURVE ( 2, ( #6275, #14758, #13007, #19727, #11564, #3195, #21500, #1540, #11448, #3306, #8272, #18175, #6621 ),
 .UNSPECIFIED., .F., .F. ) 
 B_SPLINE_CURVE_WITH_KNOTS ( ( 3, 2, 2, 2, 2, 2, 3 ),
 ( 0.4191176470588235392, 0.4205882352941176516, 0.4235294117647058765, 0.4264705882352941013, 0.4294117647058823262, 0.4323529411764706065, 0.4338235294117647189 ),
 .UNSPECIFIED. ) 
 CURVE ( )  GEOMETRIC_REPRESENTATION_ITEM ( )  RATIONAL_B_SPLINE_CURVE ( ( 0.9755282581475768211, 0.9755282581475768211, 1.000000000000000000, 0.9510565162951535312, 1.000000000000000000, 0.9510565162951535312, 1.000000000000000000, 0.9510565162951535312, 1.000000000000000000, 0.9510565162951535312, 1.000000000000000000, 0.9755282581475768211, 0.9755282581475768211 ) ) 
 REPRESENTATION_ITEM ( '' )  );
#11907 = ORIENTED_EDGE ( 'NONE', *, *, #13263, .F. ) ;
#11908 = ORIENTED_EDGE ( 'NONE', *, *, #18980, .F. ) ;
#11909 = CARTESIAN_POINT ( 'NONE',  ( 41.46631938032478359, 146.1844580088725820, 29.45539723777780239 ) ) ;
#11910 = ORIENTED_EDGE ( 'NONE', *, *, #13655, .T. ) ;
#11911 = CARTESIAN_POINT ( 'NONE',  ( 44.55648932407425633, 97.88445800887257064, 29.45539723777780239 ) ) ;
#11912 = CARTESIAN_POINT ( 'NONE',  ( 39.42975644700377558, 156.6797705074273210, 36.81289934271958941 ) ) ;
#11913 = CARTESIAN_POINT ( 'NONE',  ( 43.01140435219951286, 157.4604996726487229, 39.46799094044489209 ) ) ;
#11915 = CARTESIAN_POINT ( 'NONE',  ( 66.22715431465987024, 135.7747266163150073, -15.00590082692269078 ) ) ;
#11914 = CARTESIAN_POINT ( 'NONE',  ( 45.74753988029933538, 113.0651871740939924, 30.44471234641811819 ) ) ;
#11916 = EDGE_CURVE ( 'NONE', #15753, #14607, #13306, .T. ) ;
#11917 = CARTESIAN_POINT ( 'NONE',  ( 43.01140435219951286, 79.46049967264873715, 39.46799094044489209 ) ) ;
#11918 = CARTESIAN_POINT ( 'NONE',  ( 48.01140435219951996, 148.4344580088725536, 32.58608133808903773 ) ) ;
#11919 = CARTESIAN_POINT ( 'NONE',  ( 43.01140435219951286, 98.96049967264873715, 29.21067981925356705 ) ) ;
#11920 = CARTESIAN_POINT ( 'NONE',  ( 46.98674312866067737, 95.22448645226677399, 31.16068397573690163 ) ) ;
#11921 = CARTESIAN_POINT ( 'NONE',  ( 38.58424406990784661, 80.96518717409399812, 32.77220824515698183 ) ) ;
#11922 = DIRECTION ( 'NONE',  ( 0.000000000000000000, 1.000000000000000000, 0.000000000000000000 ) ) ;
#11923 = CARTESIAN_POINT ( 'NONE',  ( 48.01140435219951996, 121.1344580088725564, 35.83527830041810347 ) ) ;
#11924 = CARTESIAN_POINT ( 'NONE',  ( 43.01140435219951286, 107.9604996726487229, 29.21067981925356705 ) ) ;
#11925 = ORIENTED_EDGE ( 'NONE', *, *, #3680, .T. ) ;
#11926 = CARTESIAN_POINT ( 'NONE',  ( -160.8964159109769696, -191.1584106276440593, 49.65701158161630957 ) ) ;
#11927 = CARTESIAN_POINT ( 'NONE',  ( 68.29446192123552350, 96.82662215664792882, 13.41040346623746515 ) ) ;
#11928 = CARTESIAN_POINT ( 'NONE',  ( -159.0959885057557983, -173.4584106276440423, 44.11586579668791330 ) ) ;
#11929 = ORIENTED_EDGE ( 'NONE', *, *, #13773, .T. ) ;
#11930 = CARTESIAN_POINT ( 'NONE',  ( 41.64333658814960870, 156.7151871740939839, 38.42115945441014446 ) ) ;
#11931 = DIRECTION ( 'NONE',  ( -0.5010362705417042983, 0.000000000000000000, -0.8654262854811264338 ) ) ;
#11932 = CARTESIAN_POINT ( 'NONE',  ( 47.43856463449118621, 118.8797705074273239, 34.21067981925357060 ) ) ;
#11933 = CARTESIAN_POINT ( 'NONE',  ( 47.30009524607925897, 85.94413156685014599, 0.1962900075584997628 ) ) ;
#11934 = ORIENTED_EDGE ( 'NONE', *, *, #4769, .F. ) ;
#11935 = EDGE_CURVE ( 'NONE', #12008, #6487, #15418, .T. ) ;
#11936 = EDGE_CURVE ( 'NONE', #6852, #175, #11285, .T. ) ;
#11937 = VECTOR ( 'NONE', #1638, 1000.000000000000000 ) ;
#11938 = CARTESIAN_POINT ( 'NONE',  ( 66.79315400704923888, 104.7533658121278819, -7.700889860664787534 ) ) ;
#11939 = ORIENTED_EDGE ( 'NONE', *, *, #16049, .T. ) ;
#11940 = DIRECTION ( 'NONE',  ( -0.8654262854811262118, 0.000000000000000000, -0.5010362705417046314 ) ) ;
#11941 = CARTESIAN_POINT ( 'NONE',  ( -151.4692556286852607, -156.2391397928654726, 39.65701158161629536 ) ) ;
#11942 = CARTESIAN_POINT ( 'NONE',  ( 46.59305225739526435, 142.3151871740940067, 36.81289934271958941 ) ) ;
#11943 = CARTESIAN_POINT ( 'NONE',  ( 75.39856087065255963, 130.7497677300756607, 6.224699377836747871 ) ) ;
#11944 = PLANE ( 'NONE',  #14365 ) ;
#11945 = DIRECTION ( 'NONE',  ( 0.000000000000000000, 0.000000000000000000, -1.000000000000000000 ) ) ;
#11946 = CARTESIAN_POINT ( 'NONE',  ( -145.2889157411863721, -184.4391397928654328, 58.16351966513671812 ) ) ;
#11947 = CARTESIAN_POINT ( 'NONE',  ( 47.05648932407426344, 101.5104996726487485, 31.27175355779120025 ) ) ;
#11948 = LINE ( 'NONE', #12156, #20971 ) ;
#11949 = CARTESIAN_POINT ( 'NONE',  ( 47.05648932407426344, 96.98445800887257917, 37.14960608071593384 ) ) ;
#11950 = AXIS2_PLACEMENT_3D ( 'NONE', #5141, #21793, #10220 ) ;
#11951 = CARTESIAN_POINT ( 'NONE',  ( 47.43856463449117200, 98.02977050742731535, 32.77220824515698183 ) ) ;
#11952 = CARTESIAN_POINT ( 'NONE',  ( 64.66009251794113766, 101.8366349233107684, -0.5580327111990067701 ) ) ;
#11953 = CARTESIAN_POINT ( 'NONE',  ( -142.0420953463936087, -171.3938272943107393, 49.65701158161630957 ) ) ;
#11954 = CARTESIAN_POINT ( 'NONE',  ( 44.37947211624943833, 76.01518717409399528, 38.42115945441014446 ) ) ;
#11955 = CARTESIAN_POINT ( 'NONE',  ( -161.4692556286852891, -170.3391397928654669, 52.90620854394536821 ) ) ;
#11956 = DIRECTION ( 'NONE',  ( 0.000000000000000000, 0.000000000000000000, 1.000000000000000000 ) ) ;
#11957 = ORIENTED_EDGE ( 'NONE', *, *, #6105, .T. ) ;
#11958 = CARTESIAN_POINT ( 'NONE',  ( -149.8854112254399524, -190.6622583705452030, 59.65701158161632378 ) ) ;
#11959 = CYLINDRICAL_SURFACE ( 'NONE', #18364, 4.999999999999997335 ) ;
#11960 = CARTESIAN_POINT ( 'NONE',  ( 29.95680074317227692, 144.8134228754239530, -2.624813489111333720 ) ) ;
#11961 = EDGE_CURVE ( 'NONE', #12248, #1664, #9980, .T. ) ;
#11962 = EDGE_CURVE ( 'NONE', #4977, #9846, #12228, .T. ) ;
#11963 = CARTESIAN_POINT ( 'NONE',  ( 38.58424406990785371, 60.22977050742731109, 32.77220824515697473 ) ) ;
#11964 = VERTEX_POINT ( 'NONE', #18115 ) ;
#11965 = CARTESIAN_POINT ( 'NONE',  ( 44.37947211624943833, 139.2797705074273154, 38.42115945441014446 ) ) ;
#11966 =( REPRESENTATION_RELATIONSHIP ('NONE','NONE', #6933, #14632 ) REPRESENTATION_RELATIONSHIP_WITH_TRANSFORMATION ( #11508 )SHAPE_REPRESENTATION_RELATIONSHIP( ) );
#11967 = AXIS2_PLACEMENT_3D ( 'NONE', #9114, #17360, #10658 ) ;
#11968 = CARTESIAN_POINT ( 'NONE',  ( 43.01140435219953417, 142.4604996726487514, 39.21067981925356349 ) ) ;
#11969 = FACE_OUTER_BOUND ( 'NONE', #3542, .T. ) ;
#11970 = CARTESIAN_POINT ( 'NONE',  ( 131.4397495910615135, 111.2323268066561894, 14.00000000000001776 ) ) ;
#11971 = CARTESIAN_POINT ( 'NONE',  ( 162.0641828542163125, 116.7231784796025948, 4.000000000000021316 ) ) ;
#11972 = CARTESIAN_POINT ( 'NONE',  ( -151.4692556286853176, -174.8130981290893260, 59.65701158161632378 ) ) ;
#11973 = CARTESIAN_POINT ( 'NONE',  ( 43.01140435219951286, 123.5344580088725621, 39.21067981925356349 ) ) ;
#11974 = CARTESIAN_POINT ( 'NONE',  ( -141.4692556286852891, -168.2130981290892748, 52.90620854394536821 ) ) ;
#11975 = CARTESIAN_POINT ( 'NONE',  ( 47.05648932407426344, 138.9844580088725650, 37.14960608071593384 ) ) ;
#11976 = CARTESIAN_POINT ( 'NONE',  ( 39.42975644700377558, 120.0797705074273267, 31.60846029578754468 ) ) ;
#11977 = CARTESIAN_POINT ( 'NONE',  ( 69.03752116822961682, 130.9715778530742227, -2.776543650264200025 ) ) ;
#11978 = CARTESIAN_POINT ( 'NONE',  ( 41.46631938032478359, 141.3844580088725991, 38.96596240072933170 ) ) ;
#11979 = CARTESIAN_POINT ( 'NONE',  ( 43.01140435219951286, 108.8651871740939896, 38.86567161673127657 ) ) ;
#11980 = VECTOR ( 'NONE', #16201, 1000.000000000000000 ) ;
#11981 = CARTESIAN_POINT ( 'NONE',  ( 38.01140435219952707, 125.7844580088725905, 34.21067981925357060 ) ) ;
#11982 = CARTESIAN_POINT ( 'NONE',  ( 35.25059181783574758, 92.79662968204097240, -6.272318425388238694 ) ) ;
#11983 = CYLINDRICAL_SURFACE ( 'NONE', #16012, 5.000000000000004441 ) ;
#11984 = CARTESIAN_POINT ( 'NONE',  ( 46.59305225739526435, 86.17977050742732104, 31.60846029578754468 ) ) ;
#11985 = ORIENTED_EDGE ( 'NONE', *, *, #4984, .F. ) ;
#11986 = CYLINDRICAL_SURFACE ( 'NONE', #572, 4.999999999999997335 ) ;
#11987 = CARTESIAN_POINT ( 'NONE',  ( 48.01140435219951996, 70.13445800887255643, 35.83527830041810347 ) ) ;
#11988 = DIRECTION ( 'NONE',  ( 1.186952418100008983E-16, 0.000000000000000000, 1.000000000000000000 ) ) ;
#11989 = CARTESIAN_POINT ( 'NONE',  ( 46.10157429594899270, 127.7604996726487485, 38.46393386101376421 ) ) ;
#11991 = CARTESIAN_POINT ( 'NONE',  ( 69.52170837389681424, 98.37355370181180092, -13.65637406972050272 ) ) ;
#11990 = CARTESIAN_POINT ( 'NONE',  ( 43.01140435219951286, 89.36518717409398960, 29.55568802177586463 ) ) ;
#11992 = CARTESIAN_POINT ( 'NONE',  ( -143.3790856849358306, -195.6891397928654897, 43.77915905869157598 ) ) ;
#11993 = CARTESIAN_POINT ( 'NONE',  ( -148.5561028927606344, -176.7938272943107165, 40.69124936498395328 ) ) ;
#11994 = CARTESIAN_POINT ( 'NONE',  ( 38.01140435219952707, 116.9344580088725820, 35.83527830041809636 ) ) ;
#11995 = DIRECTION ( 'NONE',  ( -0.000000000000000000, 0.000000000000000000, 1.000000000000000000 ) ) ;
#11996 = DIRECTION ( 'NONE',  ( 0.000000000000000000, 1.000000000000000000, 0.000000000000000000 ) ) ;
#11997 = CARTESIAN_POINT ( 'NONE',  ( -159.5594255724347761, -173.1891397928654897, 55.53486410454104316 ) ) ;
#11998 = CARTESIAN_POINT ( 'NONE',  ( 38.58424406990784661, 153.2297705074273608, 32.77220824515698183 ) ) ;
#11999 = CARTESIAN_POINT ( 'NONE',  ( 47.43856463449117200, 107.0297705074273154, 32.77220824515698183 ) ) ;
#12000 = CARTESIAN_POINT ( 'NONE',  ( 42.88582110127141789, 154.2205544383733695, -4.165101255777401867 ) ) ;
#12001 = CARTESIAN_POINT ( 'NONE',  ( 44.37947211624943833, 137.2151871740940123, 30.00020018409699318 ) ) ;
#12002 = DIRECTION ( 'NONE',  ( 0.000000000000000000, 0.000000000000000000, 1.000000000000000000 ) ) ;
#12003 = CARTESIAN_POINT ( 'NONE',  ( -145.6429501568359797, -171.2084106276440423, 41.63779006702063867 ) ) ;
#12004 = CARTESIAN_POINT ( 'NONE',  ( 38.58424406990785371, 60.26518717409400239, 35.64915139335015937 ) ) ;
#12005 = CARTESIAN_POINT ( 'NONE',  ( 55.13406075593908895, 145.4575617026882526, 3.413969760132236964 ) ) ;
#12006 = CARTESIAN_POINT ( 'NONE',  ( 41.64333658814960870, 113.5151871740940095, 30.00020018409699318 ) ) ;
#12007 = EDGE_LOOP ( 'NONE', ( #17641, #10177, #1894, #19468 ) ) ;
#12008 = VERTEX_POINT ( 'NONE', #21552 ) ;
#12009 = CARTESIAN_POINT ( 'NONE',  ( -149.8854112254399524, -193.6622583705451461, 59.65701158161632378 ) ) ;
#12010 = ADVANCED_FACE ( 'NONE', ( #16684 ), #7888, .T. ) ;
#12011 = ORIENTED_EDGE ( 'NONE', *, *, #8895, .T. ) ;
#12012 = CARTESIAN_POINT ( 'NONE',  ( 46.10157429594899270, 102.8344580088725877, 38.46393386101376421 ) ) ;
#12013 = PRODUCT_DEFINITION_SHAPE ( 'NONE', 'NONE',  #12422 ) ;
#12014 = CARTESIAN_POINT ( 'NONE',  ( 38.58424406990786082, 159.3797705074273381, 34.21067981925357060 ) ) ;
#12015 = CARTESIAN_POINT ( 'NONE',  ( 47.43856463449117200, 62.02977050742732246, 32.77220824515698183 ) ) ;
#12017 = CARTESIAN_POINT ( 'NONE',  ( 66.60919851020621252, 104.6140855887898624, -13.69650096386476079 ) ) ;
#12016 = CARTESIAN_POINT ( 'NONE',  ( 45.74753988029933538, 112.1651871740939868, 37.97664729208901946 ) ) ;
#12018 = CARTESIAN_POINT ( 'NONE',  ( 44.55648932407425633, 76.61049967264874283, 38.96596240072933170 ) ) ;
#12019 = DIRECTION ( 'NONE',  ( -0.000000000000000000, -0.000000000000000000, -1.000000000000000000 ) ) ;
#12020 = DIRECTION ( 'NONE',  ( 0.9385982292947087080, 0.3450121214752279175, 0.000000000000000000 ) ) ;
#12021 = DIRECTION ( 'NONE',  ( 0.000000000000000000, 1.000000000000000000, 0.000000000000000000 ) ) ;
#12022 = CARTESIAN_POINT ( 'NONE',  ( 40.27526882409969033, 74.66518717409397254, 30.44471234641811819 ) ) ;
#12023 = CARTESIAN_POINT ( 'NONE',  ( 38.52630149208098942, 144.5015896161360445, 31.99467674420384355 ) ) ;
#12024 = CARTESIAN_POINT ( 'NONE',  ( -142.0420953463935803, -183.2438272943107336, 46.59394152635518793 ) ) ;
#12025 = LINE ( 'NONE', #8738, #10287 ) ;
#12026 = EDGE_CURVE ( 'NONE', #11964, #711, #6217, .T. ) ;
#12027 = VERTEX_POINT ( 'NONE', #15035 ) ;
#12028 =( BOUNDED_CURVE ( )  B_SPLINE_CURVE ( 2, ( #7082, #8847, #20631, #7516, #10819, #9058, #14217, #17197, #15454, #12244, #17306, #12571, #2218 ),
 .UNSPECIFIED., .F., .F. ) 
 B_SPLINE_CURVE_WITH_KNOTS ( ( 3, 2, 2, 2, 2, 2, 3 ),
 ( 0.5367647058823529216, 0.5382352941176470340, 0.5411764705882352589, 0.5441176470588234837, 0.5470588235294118196, 0.5500000000000000444, 0.5514705882352941568 ),
 .UNSPECIFIED. ) 
 CURVE ( )  GEOMETRIC_REPRESENTATION_ITEM ( )  RATIONAL_B_SPLINE_CURVE ( ( 0.9755282581475768211, 0.9755282581475768211, 1.000000000000000000, 0.9510565162951535312, 1.000000000000000000, 0.9510565162951535312, 1.000000000000000000, 0.9510565162951535312, 1.000000000000000000, 0.9510565162951535312, 1.000000000000000000, 0.9755282581475768211, 0.9755282581475768211 ) ) 
 REPRESENTATION_ITEM ( '' )  );
#12029 = CARTESIAN_POINT ( 'NONE',  ( -143.8425227516148084, -189.9584106276440423, 55.19815736654470584 ) ) ;
#12030 = CARTESIAN_POINT ( 'NONE',  ( 9.203281625063985061, 114.5318647093721864, 15.91056058043385413 ) ) ;
#12031 = CARTESIAN_POINT ( 'NONE',  ( -148.5561028927606344, -174.0584106276440366, 40.69124936498395328 ) ) ;
#12032 = ORIENTED_EDGE ( 'NONE', *, *, #17944, .F. ) ;
#12033 = AXIS2_PLACEMENT_3D ( 'NONE', #385, #16606, #8660 ) ;
#12034 = CARTESIAN_POINT ( 'NONE',  ( 41.64333658814960870, 153.7151871740940123, 38.42115945441014446 ) ) ;
#12035 = VECTOR ( 'NONE', #6904, 1000.000000000000000 ) ;
#12036 = DIRECTION ( 'NONE',  ( 0.000000000000000000, -1.000000000000000000, 0.000000000000000000 ) ) ;
#12037 = EDGE_CURVE ( 'NONE', #4573, #18529, #9788, .T. ) ;
#12038 = CARTESIAN_POINT ( 'NONE',  ( 38.58424406990785371, 102.5297705074273154, 35.64915139335015937 ) ) ;
#12039 = CARTESIAN_POINT ( 'NONE',  ( 25.52397925108762067, 90.47728371212039633, 7.934596195134201224 ) ) ;
#12040 = ORIENTED_EDGE ( 'NONE', *, *, #3285, .T. ) ;
#12041 = AXIS2_PLACEMENT_3D ( 'NONE', #7451, #4782, #12832 ) ;
#12042 = CARTESIAN_POINT ( 'NONE',  ( 41.15066532084431827, 91.76888749123396849, -6.510040445920065366 ) ) ;
#12043 = ORIENTED_EDGE ( 'NONE', *, *, #12037, .T. ) ;
#12044 = EDGE_CURVE ( 'NONE', #14006, #11408, #18672, .T. ) ;
#12045 = FACE_OUTER_BOUND ( 'NONE', #20267, .T. ) ;
#12046 = CARTESIAN_POINT ( 'NONE',  ( 38.01140435219952707, 128.7844580088725763, 34.21067981925357060 ) ) ;
#12047 = CARTESIAN_POINT ( 'NONE',  ( 43.01140435219951286, 143.3651871740939896, 29.55568802177586463 ) ) ;
#12048 = CARTESIAN_POINT ( 'NONE',  ( 13.69124840528610321, 102.2378096837820181, -5.517995706778950016 ) ) ;
#12049 = CARTESIAN_POINT ( 'NONE',  ( -145.2889157411863437, -180.5130981290893146, 58.16351966513671812 ) ) ;
#12050 = CARTESIAN_POINT ( 'NONE',  ( -157.6495955161842062, -173.9391397928654328, 41.15050349809590102 ) ) ;
#12051 = CARTESIAN_POINT ( 'NONE',  ( -151.4692556286852891, -182.3130981290892976, 39.65701158161629536 ) ) ;
#12052 = CYLINDRICAL_SURFACE ( 'NONE', #12163, 5.425037101889737201 ) ;
#12053 = EDGE_CURVE ( 'NONE', #21314, #15790, #19783, .T. ) ;
#12054 = CARTESIAN_POINT ( 'NONE',  ( 45.74753988029933538, 82.42977050742732104, 37.97664729208901946 ) ) ;
#12055 = CARTESIAN_POINT ( 'NONE',  ( 66.16974147772015158, 135.9983230778657344, -9.010293137571032673 ) ) ;
#12056 = CARTESIAN_POINT ( 'NONE',  ( -145.6429501568359797, -177.8438272943106995, 57.67623309621198047 ) ) ;
#12057 = CARTESIAN_POINT ( 'NONE',  ( 39.42975644700377558, 81.41518717409400097, 36.81289934271958941 ) ) ;
#12058 = LINE ( 'NONE', #6478, #8888 ) ;
#12059 = CARTESIAN_POINT ( 'NONE',  ( -154.5594255724347761, -157.8891397928654783, 59.16757674456785310 ) ) ;
#12060 = EDGE_LOOP ( 'NONE', ( #6122, #17849 ) ) ;
#12061 = CARTESIAN_POINT ( 'NONE',  ( -154.5594255724347761, -176.1630981290893203, 40.14644641866476604 ) ) ;
#12062 = EDGE_CURVE ( 'NONE', #3065, #8092, #1371, .T. ) ;
#12063 = CARTESIAN_POINT ( 'NONE',  ( 44.55648932407425633, 122.8104996726487457, 29.45539723777780239 ) ) ;
#12064 = CARTESIAN_POINT ( 'NONE',  ( 46.59305225739526435, 142.5797705074273267, 36.81289934271958941 ) ) ;
#12065 = CARTESIAN_POINT ( 'NONE',  ( 29.68407903333335085, 144.6596297928226988, 11.33750686376150085 ) ) ;
#12066 = ORIENTED_EDGE ( 'NONE', *, *, #3557, .T. ) ;
#12067 = CARTESIAN_POINT ( 'NONE',  ( 43.01140435219951286, 120.5344580088725763, 39.21067981925356349 ) ) ;
#12068 = ORIENTED_EDGE ( 'NONE', *, *, #827, .T. ) ;
#12069 = CARTESIAN_POINT ( 'NONE',  ( 47.43856463449118621, 133.8797705074273381, 34.21067981925357060 ) ) ;
#12070 = EDGE_CURVE ( 'NONE', #15353, #9281, #6443, .T. ) ;
#12071 = CARTESIAN_POINT ( 'NONE',  ( 40.27526882409969033, 62.66518717409400097, 30.44471234641811819 ) ) ;
#12072 = FACE_OUTER_BOUND ( 'NONE', #675, .T. ) ;
#12073 = CARTESIAN_POINT ( 'NONE',  ( 43.01140435219951286, 126.5344580088725621, 39.21067981925356349 ) ) ;
#12074 = CARTESIAN_POINT ( 'NONE',  ( 47.43856463449118621, 100.6151871740940180, 34.21067981925357060 ) ) ;
#12075 = CARTESIAN_POINT ( 'NONE',  ( 38.96631938032478359, 154.0104996726487343, 37.14960608071593384 ) ) ;
#12076 = CARTESIAN_POINT ( 'NONE',  ( 41.46631938032478359, 122.1844580088725962, 29.45539723777780239 ) ) ;
#12077 = CARTESIAN_POINT ( 'NONE',  ( -159.5594255724347761, -172.8630981290893089, 43.77915905869157598 ) ) ;
#12078 = CARTESIAN_POINT ( 'NONE',  ( 0.000000000000000000, 0.000000000000000000, -33.99999999999999289 ) ) ;
#12079 = CARTESIAN_POINT ( 'NONE',  ( -161.4692556286853176, -191.4891397928654726, 49.65701158161630957 ) ) ;
#12080 = CARTESIAN_POINT ( 'NONE',  ( 38.96631938032478359, 138.0844580088725877, 37.14960608071593384 ) ) ;
#12081 = CARTESIAN_POINT ( 'NONE',  ( 47.43856463449118621, 124.8797705074273239, 34.21067981925357060 ) ) ;
#12082 = CARTESIAN_POINT ( 'NONE',  ( 61.02373258766779429, 98.10483126312279012, -1.347972122102980119 ) ) ;
#12083 = CARTESIAN_POINT ( 'NONE',  ( 39.92123440845005433, 140.3344580088725877, 29.95742577749336988 ) ) ;
#12084 = CARTESIAN_POINT ( 'NONE',  ( 46.59305225739526435, 103.3151871740940067, 36.81289934271958941 ) ) ;
#12085 = CARTESIAN_POINT ( 'NONE',  ( 38.96631938032478359, 126.0844580088725735, 37.14960608071593384 ) ) ;
#12086 = CARTESIAN_POINT ( 'NONE',  ( 9.997522862669264043, 111.1595821513141402, 9.795857695845493041 ) ) ;
#12087 = CARTESIAN_POINT ( 'NONE',  ( 59.36841858216658352, 96.93634223693318575, 13.72768157422830981 ) ) ;
#12088 = FACE_OUTER_BOUND ( 'NONE', #9448, .T. ) ;
#12089 = CARTESIAN_POINT ( 'NONE',  ( 41.64333658814960870, 84.97977050742731819, 38.42115945441014446 ) ) ;
#12090 = CARTESIAN_POINT ( 'NONE',  ( 43.80332655382221674, 110.8836182503284675, 29.21067981925357060 ) ) ;
#12091 = CARTESIAN_POINT ( 'NONE',  ( 38.01140435219952707, 71.78445800887257633, 34.21067981925357060 ) ) ;
#12092 = PLANE ( 'NONE',  #18275 ) ;
#12093 = CARTESIAN_POINT ( 'NONE',  ( 47.05648932407426344, 134.5104996726487343, 31.27175355779120025 ) ) ;
#12095 = CARTESIAN_POINT ( 'NONE',  ( 36.78388215320455856, 153.4884242111695301, -9.370659782632428048 ) ) ;
#12094 = CARTESIAN_POINT ( 'NONE',  ( 44.37947211624943833, 91.01518717409399528, 38.42115945441014446 ) ) ;
#12096 = CARTESIAN_POINT ( 'NONE',  ( -160.8964159109769696, -158.1584106276440593, 49.65701158161630957 ) ) ;
#12097 = EDGE_CURVE ( 'NONE', #6852, #16883, #378, .T. ) ;
#12098 = CARTESIAN_POINT ( 'NONE',  ( -159.0959885057557983, -184.5938272943107279, 55.19815736654470584 ) ) ;
#12099 = CARTESIAN_POINT ( 'NONE',  ( -151.4692556286852891, -177.2391397928654442, 39.65701158161629536 ) ) ;
#12100 = CYLINDRICAL_SURFACE ( 'NONE', #16343, 10.00000000000000888 ) ;
#12101 =( LENGTH_UNIT ( ) NAMED_UNIT ( * ) SI_UNIT ( .MILLI., .METRE. ) );
#12102 = CARTESIAN_POINT ( 'NONE',  ( 41.46631938032478359, 92.18445800887258201, 29.45539723777780239 ) ) ;
#12103 = CARTESIAN_POINT ( 'NONE',  ( 43.01140435219953417, 142.4604996726487514, 39.21067981925356349 ) ) ;
#12104 = CARTESIAN_POINT ( 'NONE',  ( 40.27526882409969033, 149.9297705074272926, 30.44471234641811819 ) ) ;
#12105 = CARTESIAN_POINT ( 'NONE',  ( 43.01140435219951286, 106.1297705074272955, 38.86567161673127657 ) ) ;
#12106 = CARTESIAN_POINT ( 'NONE',  ( 16.30372524420941716, 141.3216567370616019, 9.839263250375132941 ) ) ;
#12107 = CARTESIAN_POINT ( 'NONE',  ( 47.43856463449117911, 139.4651871740940123, 35.64915139335015937 ) ) ;
#12108 = CARTESIAN_POINT ( 'NONE',  ( 43.80332655382220253, 66.61133943119283174, 39.21067981925355639 ) ) ;
#12109 = CARTESIAN_POINT ( 'NONE',  ( -151.4692556286852891, -161.9084106276440593, 39.74470866294723947 ) ) ;
#12110 = CARTESIAN_POINT ( 'NONE',  ( 47.05648932407426344, 90.98445800887257917, 37.14960608071593384 ) ) ;
#12111 = AXIS2_PLACEMENT_3D ( 'NONE', #5282, #11996, #3956 ) ;
#12112 = CARTESIAN_POINT ( 'NONE',  ( 66.97710950389229367, 104.8926460354658587, -1.705278757464820938 ) ) ;
#12113 = DIRECTION ( 'NONE',  ( -0.000000000000000000, -0.000000000000000000, -1.000000000000000000 ) ) ;
#12114 = CARTESIAN_POINT ( 'NONE',  ( 46.59305225739526435, 115.3151871740940067, 36.81289934271958941 ) ) ;
#12115 = ORIENTED_EDGE ( 'NONE', *, *, #20597, .F. ) ;
#12116 = CARTESIAN_POINT ( 'NONE',  ( -159.5594255724347761, -179.1891397928654612, 55.53486410454104316 ) ) ;
#12117 = ORIENTED_EDGE ( 'NONE', *, *, #13885, .F. ) ;
#12118 = CARTESIAN_POINT ( 'NONE',  ( 38.01140435219952707, 104.7844580088725763, 34.21067981925357060 ) ) ;
#12119 = CARTESIAN_POINT ( 'NONE',  ( 43.01140435219951286, 155.9604996726487229, 28.95336869806222779 ) ) ;
#12121 = CARTESIAN_POINT ( 'NONE',  ( 43.96673757894181023, 91.80305570246190427, -12.62481348914368873 ) ) ;
#12120 = CARTESIAN_POINT ( 'NONE',  ( 41.64333658814960870, 116.5151871740940095, 30.00020018409699318 ) ) ;
#12122 = AXIS2_PLACEMENT_3D ( 'NONE', #20046, #10114, #18263 ) ;
#12123 = CARTESIAN_POINT ( 'NONE',  ( 38.01140435219951996, 69.86049967264871441, 35.83527830041810347 ) ) ;
#12125 = CARTESIAN_POINT ( 'NONE',  ( 47.05648932407426344, 135.9844580088725934, 37.14960608071593384 ) ) ;
#12124 = CARTESIAN_POINT ( 'NONE',  ( 151.4773229304660731, 84.89323405393692212, 4.000000000000021316 ) ) ;
#12126 = CARTESIAN_POINT ( 'NONE',  ( -154.5594255724347761, -171.9630981290893033, 59.16757674456785310 ) ) ;
#12127 = CARTESIAN_POINT ( 'NONE',  ( 47.97937126593587465, 95.40557542420955883, 34.86469163422184181 ) ) ;
#12128 = CARTESIAN_POINT ( 'NONE',  ( 40.27526882409969033, 78.56518717409399244, 37.97664729208901946 ) ) ;
#12129 = CARTESIAN_POINT ( 'NONE',  ( 42.21948215057684450, 64.38361825032846752, 39.21067981925355639 ) ) ;
#12130 = CARTESIAN_POINT ( 'NONE',  ( -154.3824083646099439, -178.2938272943107165, 58.62277379824867296 ) ) ;
#12131 = CARTESIAN_POINT ( 'NONE',  ( 5.130598475945862827E-15, 0.000000000000000000, 10.00000000000001599 ) ) ;
#12132 = VERTEX_POINT ( 'NONE', #8868 ) ;
#12133 = CARTESIAN_POINT ( 'NONE',  ( -143.8425227516148084, -186.3584106276440480, 44.11586579668791330 ) ) ;
#12134 = CARTESIAN_POINT ( 'NONE',  ( 74.27779736592162863, 105.9683817680885056, 13.05343286460986363 ) ) ;
#12135 = ORIENTED_EDGE ( 'NONE', *, *, #8887, .T. ) ;
#12136 = CARTESIAN_POINT ( 'NONE',  ( 44.37947211624943833, 145.0151871740939953, 38.42115945441014446 ) ) ;
#12137 = CARTESIAN_POINT ( 'NONE',  ( -151.4692556286852891, -126.9891397928655010, 39.65701158161630246 ) ) ;
#12138 = CARTESIAN_POINT ( 'NONE',  ( 47.43856463449118621, 103.8797705074273239, 34.21067981925357060 ) ) ;
#12139 = CARTESIAN_POINT ( 'NONE',  ( 12.03843011909301453, 134.4860913190374561, 2.577281550626734141 ) ) ;
#12140 = VERTEX_POINT ( 'NONE', #7107 ) ;
#12141 = CARTESIAN_POINT ( 'NONE',  ( 42.95897134029118547, 91.70801217734280897, 7.418363685804686192 ) ) ;
#12142 = ORIENTED_EDGE ( 'NONE', *, *, #15076, .T. ) ;
#12143 = CARTESIAN_POINT ( 'NONE',  ( 38.58424406990784661, 111.2297705074273324, 32.77220824515698183 ) ) ;
#12144 = CARTESIAN_POINT ( 'NONE',  ( -23.27144139456156324, -18.88988604584387332, -19.99999999999997868 ) ) ;
#12145 = CARTESIAN_POINT ( 'NONE',  ( 42.21948215057684450, 127.3836182503284533, 39.21067981925355639 ) ) ;
#12146 = AXIS2_PLACEMENT_3D ( 'NONE', #20587, #17586, #17371 ) ;
#12147 = EDGE_CURVE ( 'NONE', #4877, #10397, #5207, .T. ) ;
#12148 = CARTESIAN_POINT ( 'NONE',  ( 47.43856463449118621, 148.6151871740939896, 34.21067981925357060 ) ) ;
#12149 = CARTESIAN_POINT ( 'NONE',  ( 38.96631938032478359, 103.0104996726487485, 37.14960608071593384 ) ) ;
#12150 = CARTESIAN_POINT ( 'NONE',  ( 66.89036333300305159, 144.4373801540182569, -2.303882249869787291 ) ) ;
#12151 = CARTESIAN_POINT ( 'NONE',  ( -39.63192160874135084, -354.7018910364275257, 20.00000000000002132 ) ) ;
#12152 = CARTESIAN_POINT ( 'NONE',  ( -143.3790856849358306, -166.2891397928654840, 55.53486410454105027 ) ) ;
#12153 =( BOUNDED_CURVE ( )  B_SPLINE_CURVE ( 2, ( #16817, #1730, #8464, #15283, #15171, #74, #13518, #20251, #18593, #178, #5253, #7238, #10543 ),
 .UNSPECIFIED., .F., .F. ) 
 B_SPLINE_CURVE_WITH_KNOTS ( ( 3, 2, 2, 2, 2, 2, 3 ),
 ( 0.5892857142857143016, 0.5928571428571428603, 0.5999999999999999778, 0.6071428571428570953, 0.6142857142857143238, 0.6214285714285714413, 0.6250000000000000000 ),
 .UNSPECIFIED. ) 
 CURVE ( )  GEOMETRIC_REPRESENTATION_ITEM ( )  RATIONAL_B_SPLINE_CURVE ( ( 0.9755282581475768211, 0.9755282581475768211, 1.000000000000000000, 0.9510565162951535312, 1.000000000000000000, 0.9510565162951535312, 1.000000000000000000, 0.9510565162951535312, 1.000000000000000000, 0.9510565162951535312, 1.000000000000000000, 0.9755282581475768211, 0.9755282581475768211 ) ) 
 REPRESENTATION_ITEM ( '' )  );
#12154 = EDGE_CURVE ( 'NONE', #14607, #15753, #18226, .T. ) ;
#12155 = CARTESIAN_POINT ( 'NONE',  ( 43.01140435219951996, 10.71049967264875491, 34.21067981925357060 ) ) ;
#12156 = CARTESIAN_POINT ( 'NONE',  ( 43.01140435219951996, 10.71049967264875491, 39.21067981925356349 ) ) ;
#12157 = CARTESIAN_POINT ( 'NONE',  ( 43.01140435219951286, 152.0344580088725763, 29.21067981925356705 ) ) ;
#12158 = DIRECTION ( 'NONE',  ( -0.000000000000000000, -0.000000000000000000, -1.000000000000000000 ) ) ;
#12159 = CARTESIAN_POINT ( 'NONE',  ( 47.43856463449117200, 83.02977050742730114, 32.77220824515698183 ) ) ;
#12160 = CARTESIAN_POINT ( 'NONE',  ( -160.8964159109769696, -175.7438272943107052, 52.72008163687743121 ) ) ;
#12161 = CARTESIAN_POINT ( 'NONE',  ( 134.6380592378700101, 268.5785371414991687, -19.99999999999997868 ) ) ;
#12162 = CARTESIAN_POINT ( 'NONE',  ( 130.1509106190733007, 127.1041540266590602, 272.0939500981630204 ) ) ;
#12163 = AXIS2_PLACEMENT_3D ( 'NONE', #20442, #18782, #7002 ) ;
#12164 = ORIENTED_EDGE ( 'NONE', *, *, #17476, .F. ) ;
#12165 = CARTESIAN_POINT ( 'NONE',  ( 39.92123440845005433, 68.33445800887258770, 29.95742577749336988 ) ) ;
#12166 = CARTESIAN_POINT ( 'NONE',  ( 43.80332655382220253, 121.5373810949690068, 39.21067981925355639 ) ) ;
#12167 = CARTESIAN_POINT ( 'NONE',  ( 43.01140435219951286, 131.6297705074273381, 29.55568802177586107 ) ) ;
#12168 = CARTESIAN_POINT ( 'NONE',  ( 33.24893159794274311, 146.2783277815063059, 4.518043653832040540 ) ) ;
#12169 = ORIENTED_EDGE ( 'NONE', *, *, #192, .T. ) ;
#12170 = CARTESIAN_POINT ( 'NONE',  ( 38.96631938032478359, 119.4844580088725792, 31.27175355779120025 ) ) ;
#12171 = ORIENTED_EDGE ( 'NONE', *, *, #21718, .T. ) ;
#12172 = CARTESIAN_POINT ( 'NONE',  ( 39.42975644700377558, 132.0797705074273267, 31.60846029578754468 ) ) ;
#12173 = CARTESIAN_POINT ( 'NONE',  ( 45.74753988029933538, 91.42977050742732104, 37.97664729208901946 ) ) ;
#12174 = CARTESIAN_POINT ( 'NONE',  ( 47.05648932407426344, 155.5104996726487343, 31.27175355779120025 ) ) ;
#12175 = VECTOR ( 'NONE', #7769, 1000.000000000000000 ) ;
#12176 = DIRECTION ( 'NONE',  ( 8.659560562354814529E-17, 0.7071067811865573427, -0.7071067811865378028 ) ) ;
#12177 = FILL_AREA_STYLE ('',( #19024 ) ) ;
#12178 = AXIS2_PLACEMENT_3D ( 'NONE', #21434, #14695, #6550 ) ;
#12179 = EDGE_CURVE ( 'NONE', #8778, #12631, #5122, .T. ) ;
#12180 = CARTESIAN_POINT ( 'NONE',  ( 38.58424406990784661, 93.26518717409399528, 35.64915139335016647 ) ) ;
#12181 = CARTESIAN_POINT ( 'NONE',  ( 43.01140435219951996, 119.9070776186055838, 50.00000000000002842 ) ) ;
#12182 = CARTESIAN_POINT ( 'NONE',  ( 43.01140435219951286, 146.9604996726487229, 29.21067981925356705 ) ) ;
#12183 = CARTESIAN_POINT ( 'NONE',  ( -151.4692556286852891, -168.8130981290893260, 60.17163382399899518 ) ) ;
#12184 = CARTESIAN_POINT ( 'NONE',  ( -161.4692556286852891, -191.3391397928654669, 52.90620854394536821 ) ) ;
#12185 = CARTESIAN_POINT ( 'NONE',  ( 44.55648932407425633, 144.6844580088725820, 38.96596240072933170 ) ) ;
#12186 = CARTESIAN_POINT ( 'NONE',  ( 43.01140435219951286, 109.1297705074273239, 38.86567161673127657 ) ) ;
#12187 = CARTESIAN_POINT ( 'NONE',  ( 24.80496442426440140, 98.26638142913259344, 0.1995735771552373528 ) ) ;
#12188 = CARTESIAN_POINT ( 'NONE',  ( 173.3794444120442506, -34.13255853780189142, 5.000000000000018652 ) ) ;
#12189 = CARTESIAN_POINT ( 'NONE',  ( 47.43856463449117911, 109.7651871740940095, 32.77220824515697473 ) ) ;
#12190 = ORIENTED_EDGE ( 'NONE', *, *, #14444, .T. ) ;
#12191 = CARTESIAN_POINT ( 'NONE',  ( 156.7804311855217065, 208.8003142469820830, -44.99999999999997158 ) ) ;
#12192 = CARTESIAN_POINT ( 'NONE',  ( 8.944919112598912037, 123.2842988173194385, -4.803623532975393573 ) ) ;
#12193 = ADVANCED_FACE ( 'NONE', ( #3360 ), #17009, .T. ) ;
#12194 = AXIS2_PLACEMENT_3D ( 'NONE', #2752, #12676, #21280 ) ;
#12195 = CARTESIAN_POINT ( 'NONE',  ( 51.29519266978688563, 92.95216133272363379, 14.08499220319455780 ) ) ;
#12196 = DIRECTION ( 'NONE',  ( -0.7067093775913380060, 0.7073806645723110798, -0.01320799052465155242 ) ) ;
#12197 = CARTESIAN_POINT ( 'NONE',  ( 43.01140435219951286, 88.12977050742732388, 38.86567161673127657 ) ) ;
#12198 = AXIS2_PLACEMENT_3D ( 'NONE', #10862, #8990, #9312 ) ;
#12199 = ORIENTED_EDGE ( 'NONE', *, *, #14114, .T. ) ;
#12200 = EDGE_CURVE ( 'NONE', #10861, #1573, #11884, .T. ) ;
#12201 = B_SPLINE_CURVE_WITH_KNOTS ( 'NONE', 3,
 ( #21304, #17651, #4535, #1345, #17867, #11255, #20977, #19755, #19528, #12808, #4649, #2996, #11368, #11042, #9519, #9625, #21195, #6081, #9735, #5865, #12919, #14562, #12596, #4215, #2558, #17758, #16324, #9295, #7651, #19644, #21091, #1128, #5972, #12700, #2660, #19421, #7756, #4422 ),
 .UNSPECIFIED., .F., .F.,
 ( 4, 2, 2, 2, 2, 2, 2, 2, 2, 2, 2, 2, 2, 2, 2, 2, 2, 2, 4 ),
 ( 0.01567185795944685614, 0.01665109603395603308, 0.01763033410846520654, 0.01811995314571980542, 0.01860957218297440430, 0.01958881025748360205, 0.02056804833199280327, 0.02154728640650200797, 0.02252652448101120919, 0.02350576255552041388, 0.02448500063002961857, 0.02546423870453881980, 0.02644347677904802449, 0.02693309581630264071, 0.02742271485355725694, 0.02840195292806652061, 0.02938119100257578775, 0.03036042907708504796, 0.03133966715159431510 ),
 .UNSPECIFIED. ) ;
#12202 = CARTESIAN_POINT ( 'NONE',  ( 44.55648932407425633, 73.88445800887258486, 29.45539723777780239 ) ) ;
#12203 = CARTESIAN_POINT ( 'NONE',  ( -151.4692556286852607, -171.2391397928654726, 39.65701158161629536 ) ) ;
#12204 = CARTESIAN_POINT ( 'NONE',  ( 48.01140435219951996, 128.3604996726487286, 32.58608133808903773 ) ) ;
#12206 = CARTESIAN_POINT ( 'NONE',  ( 20.63953418349755253, 94.10117616956034681, -11.87063135391590052 ) ) ;
#12205 = CARTESIAN_POINT ( 'NONE',  ( 38.58424406990784661, 90.26518717409398107, 35.64915139335016647 ) ) ;
#12207 = CARTESIAN_POINT ( 'NONE',  ( -154.5594255724347761, -195.0891397928654669, 40.14644641866476604 ) ) ;
#12208 = CARTESIAN_POINT ( 'NONE',  ( -154.3824083646099439, -184.2938272943107449, 58.62277379824867296 ) ) ;
#12209 = CARTESIAN_POINT ( 'NONE',  ( 39.92123440845005433, 94.16049967264872578, 38.46393386101375711 ) ) ;
#12210 = CARTESIAN_POINT ( 'NONE',  ( 43.80332655382220253, 126.6113394311928460, 39.21067981925355639 ) ) ;
#12211 =( LENGTH_UNIT ( ) NAMED_UNIT ( * ) SI_UNIT ( .MILLI., .METRE. ) );
#12212 = FACE_BOUND ( 'NONE', #1636, .T. ) ;
#12213 = LINE ( 'NONE', #15315, #5503 ) ;
#12214 = CARTESIAN_POINT ( 'NONE',  ( 40.27526882409969033, 146.9297705074273210, 30.44471234641811819 ) ) ;
#12215 = CARTESIAN_POINT ( 'NONE',  ( 39.42975644700377558, 102.0797705074273267, 31.60846029578754468 ) ) ;
#12216 = CARTESIAN_POINT ( 'NONE',  ( 70.62757080055673953, 99.67629488849819097, 13.29148015538516425 ) ) ;
#12217 = CARTESIAN_POINT ( 'NONE',  ( 45.74753988029934249, 134.0651871740939498, 30.44471234641812174 ) ) ;
#12218 = CARTESIAN_POINT ( 'NONE',  ( 43.01140435219951996, 170.7104996726487514, 34.21067981925357060 ) ) ;
#12219 = CARTESIAN_POINT ( 'NONE',  ( -142.0420953463935803, -165.8084106276440366, 52.72008163687743831 ) ) ;
#12220 = CARTESIAN_POINT ( 'NONE',  ( 47.43856463449117200, 64.72977050742731819, 35.64915139335016647 ) ) ;
#12221 = LINE ( 'NONE', #2092, #68 ) ;
#12222 =( BOUNDED_CURVE ( )  B_SPLINE_CURVE ( 2, ( #6866, #16660, #24, #20205, #15456, #5098, #10064, #15007, #15347, #13572, #10392, #356, #1893 ),
 .UNSPECIFIED., .F., .F. ) 
 B_SPLINE_CURVE_WITH_KNOTS ( ( 3, 2, 2, 2, 2, 2, 3 ),
 ( 0.2573529411764705621, 0.2588235294117647300, 0.2617647058823529549, 0.2647058823529411797, 0.2676470588235294046, 0.2705882352941176294, 0.2720588235294117974 ),
 .UNSPECIFIED. ) 
 CURVE ( )  GEOMETRIC_REPRESENTATION_ITEM ( )  RATIONAL_B_SPLINE_CURVE ( ( 0.9755282581475768211, 0.9755282581475763770, 1.000000000000000000, 0.9510565162951535312, 1.000000000000000000, 0.9510565162951535312, 1.000000000000000000, 0.9510565162951535312, 1.000000000000000000, 0.9510565162951535312, 1.000000000000000000, 0.9755282581475763770, 0.9755282581475768211 ) ) 
 REPRESENTATION_ITEM ( '' )  );
#12223 = CARTESIAN_POINT ( 'NONE',  ( 14.82355424275916000, 117.6079223783217458, 15.08068057431173870 ) ) ;
#12224 = CIRCLE ( 'NONE', #3087, 88.09373137032866907 ) ;
#12225 =( LENGTH_UNIT ( ) NAMED_UNIT ( * ) SI_UNIT ( .MILLI., .METRE. ) );
#12226 = CARTESIAN_POINT ( 'NONE',  ( 47.43856463449118621, 118.6151871740940038, 34.21067981925357060 ) ) ;
#12227 = ORIENTED_EDGE ( 'NONE', *, *, #4382, .T. ) ;
#12228 = CIRCLE ( 'NONE', #3094, 10.00000000000000888 ) ;
#12229 = EDGE_CURVE ( 'NONE', #8, #21213, #17809, .T. ) ;
#12230 = CARTESIAN_POINT ( 'NONE',  ( 43.01140435219951286, 76.46049967264873715, 39.21067981925356349 ) ) ;
#12231 = ORIENTED_EDGE ( 'NONE', *, *, #15022, .T. ) ;
#12232 = CARTESIAN_POINT ( 'NONE',  ( 48.01140435219951996, 106.1344580088725849, 35.83527830041810347 ) ) ;
#12233 = CARTESIAN_POINT ( 'NONE',  ( 38.58424406990785371, 150.5297705074272869, 35.64915139335015937 ) ) ;
#12234 = CARTESIAN_POINT ( 'NONE',  ( 45.22505347682931642, 59.38050100342833559, 30.37668637662400073 ) ) ;
#12236 = CARTESIAN_POINT ( 'NONE',  ( 23.35610682547305927, 99.68565781958278649, 15.27541961222430444 ) ) ;
#12235 = CARTESIAN_POINT ( 'NONE',  ( 43.01140435219951286, 111.8651871740939896, 38.86567161673127657 ) ) ;
#12237 = VECTOR ( 'NONE', #10123, 1000.000000000000000 ) ;
#12238 = CARTESIAN_POINT ( 'NONE',  ( 47.05648932407426344, 71.51049967264873430, 31.27175355779120025 ) ) ;
#12240 = CARTESIAN_POINT ( 'NONE',  ( 47.05648932407426344, 136.5844580088725877, 31.27175355779120025 ) ) ;
#12239 = CARTESIAN_POINT ( 'NONE',  ( 46.06326223953917065, 144.7216122669715332, 30.23659822568390965 ) ) ;
#12241 = CARTESIAN_POINT ( 'NONE',  ( 43.01140435219951286, 124.4604996726487371, 39.21067981925356349 ) ) ;
#12242 = DIRECTION ( 'NONE',  ( -1.000000000000000000, 0.000000000000000000, 0.000000000000000000 ) ) ;
#12243 = CARTESIAN_POINT ( 'NONE',  ( 38.58424406990784661, 81.26518717409398107, 35.64915139335016647 ) ) ;
#12244 = CARTESIAN_POINT ( 'NONE',  ( 46.10157429594899270, 103.7604996726487485, 38.46393386101375711 ) ) ;
#12245 = VECTOR ( 'NONE', #16083, 1000.000000000000000 ) ;
#12246 = CARTESIAN_POINT ( 'NONE',  ( -160.8964159109769696, -178.7438272943107052, 52.72008163687743121 ) ) ;
#12247 = CARTESIAN_POINT ( 'NONE',  ( 45.22505347682923116, 59.38050100342834270, 30.37668637662395099 ) ) ;
#12248 = VERTEX_POINT ( 'NONE', #17218 ) ;
#12249 = CARTESIAN_POINT ( 'NONE',  ( 8.867590775667826719, 116.4845415224344833, 7.977433149383395872 ) ) ;
#12250 = EDGE_LOOP ( 'NONE', ( #1831, #20399, #14015, #15592 ) ) ;
#12251 = CARTESIAN_POINT ( 'NONE',  ( 39.42975644700377558, 146.8151871740940067, 31.60846029578754468 ) ) ;
#12252 = DIRECTION ( 'NONE',  ( -1.000000000000000000, 0.000000000000000000, 0.000000000000000000 ) ) ;
#12253 = CARTESIAN_POINT ( 'NONE',  ( 44.37947211624943833, 103.2797705074273154, 38.42115945441014446 ) ) ;
#12254 = CARTESIAN_POINT ( 'NONE',  ( 67.39040179371399120, 143.9404232637865562, 4.720051584306741432 ) ) ;
#12255 = VERTEX_POINT ( 'NONE', #18780 ) ;
#12256 = CARTESIAN_POINT ( 'NONE',  ( 15.53003795322992353, 126.2325256570730687, 2.418278830334454899 ) ) ;
#12257 = ORIENTED_EDGE ( 'NONE', *, *, #5437, .T. ) ;
#12258 = CARTESIAN_POINT ( 'NONE',  ( 47.43856463449117200, 112.7297705074273182, 35.64915139335016647 ) ) ;
#12259 = CARTESIAN_POINT ( 'NONE',  ( 43.01140435219952707, 144.9070776186055696, 39.21067981925356349 ) ) ;
#12260 = CARTESIAN_POINT ( 'NONE',  ( 139.9279279298906147, 262.8829071470230474, 4.000000000000012434 ) ) ;
#12261 = CARTESIAN_POINT ( 'NONE',  ( 43.01140435219951286, 140.3651871740940180, 29.55568802177586463 ) ) ;
#12262 = CARTESIAN_POINT ( 'NONE',  ( 47.05648932407426344, 101.5104996726487485, 31.27175355779120025 ) ) ;
#12263 = CARTESIAN_POINT ( 'NONE',  ( 47.30009524607925897, 85.94413156685014599, 0.1962900075584997628 ) ) ;
#12264 = CARTESIAN_POINT ( 'NONE',  ( 136.1800780017398722, 182.0764489627892715, 20.08191530401613178 ) ) ;
#12265 = CARTESIAN_POINT ( 'NONE',  ( -157.6495955161842062, -167.9391397928654897, 41.15050349809590102 ) ) ;
#12266 = DIRECTION ( 'NONE',  ( 0.000000000000000000, 0.000000000000000000, -1.000000000000000000 ) ) ;
#12267 = CARTESIAN_POINT ( 'NONE',  ( 44.55648932407425633, 63.68445800887258201, 38.96596240072933170 ) ) ;
#12268 = CARTESIAN_POINT ( 'NONE',  ( 43.01140435219951996, 10.71049967264875491, 29.21067981925357060 ) ) ;
#12269 = CARTESIAN_POINT ( 'NONE',  ( 41.64333658814960870, 84.97977050742731819, 38.42115945441014446 ) ) ;
#12270 = CARTESIAN_POINT ( 'NONE',  ( -160.8964159109769696, -160.8938272943107393, 49.65701158161630957 ) ) ;
#12271 = CARTESIAN_POINT ( 'NONE',  ( 39.42975644700377558, 78.41518717409400097, 36.81289934271958941 ) ) ;
#12272 = DIRECTION ( 'NONE',  ( 0.3450121214752279175, -0.9385982292947087080, 0.000000000000000000 ) ) ;
#12273 = LINE ( 'NONE', #10530, #20984 ) ;
#12274 = ORIENTED_EDGE ( 'NONE', *, *, #14566, .T. ) ;
#12275 = CARTESIAN_POINT ( 'NONE',  ( 46.10157429594899270, 84.83445800887258770, 38.46393386101375711 ) ) ;
#12276 = DIRECTION ( 'NONE',  ( 0.3450121214752278620, -0.9385982292947087080, 0.000000000000000000 ) ) ;
#12277 = CARTESIAN_POINT ( 'NONE',  ( 38.58424406990785371, 129.5297705074273154, 35.64915139335015937 ) ) ;
#12278 = CARTESIAN_POINT ( 'NONE',  ( 65.51498131554875215, 136.7693945797108199, 5.946615082358765569 ) ) ;
#12279 = VERTEX_POINT ( 'NONE', #8437 ) ;
#12280 = CARTESIAN_POINT ( 'NONE',  ( 47.05648932407426344, 72.98445800887257917, 37.14960608071593384 ) ) ;
#12281 = VERTEX_POINT ( 'NONE', #2136 ) ;
#12282 = CARTESIAN_POINT ( 'NONE',  ( 44.37947211624943833, 134.4797705074273324, 30.00020018409699318 ) ) ;
#12283 = CIRCLE ( 'NONE', #3856, 10.00000000000000888 ) ;
#12284 = DIRECTION ( 'NONE',  ( 0.000000000000000000, 0.000000000000000000, 1.000000000000000000 ) ) ;
#12285 = CARTESIAN_POINT ( 'NONE',  ( 38.96631938032478359, 129.4104996726487684, 31.27175355779120025 ) ) ;
#12286 = LINE ( 'NONE', #15808, #1394 ) ;
#12287 = CARTESIAN_POINT ( 'NONE',  ( 47.43856463449117200, 94.76518717409398107, 32.77220824515698183 ) ) ;
#12288 = CARTESIAN_POINT ( 'NONE',  ( -142.0420953463936087, -156.3938272943107393, 49.65701158161630957 ) ) ;
#12289 = DIRECTION ( 'NONE',  ( -0.000000000000000000, -0.000000000000000000, -1.000000000000000000 ) ) ;
#12290 = CARTESIAN_POINT ( 'NONE',  ( -143.3790856849358306, -162.3630981290893089, 55.53486410454105027 ) ) ;
#12291 = CARTESIAN_POINT ( 'NONE',  ( -151.4692556286852891, -190.7391397928654726, 59.65701158161632378 ) ) ;
#12292 = CARTESIAN_POINT ( 'NONE',  ( 47.05648932407426344, 130.5844580088725877, 31.27175355779120025 ) ) ;
#12293 = CARTESIAN_POINT ( 'NONE',  ( 47.43856463449118621, 109.8797705074273239, 34.21067981925357060 ) ) ;
#12294 = CARTESIAN_POINT ( 'NONE',  ( 26.46568392313936968, 149.8720644322279725, 23.30118661649528633 ) ) ;
#12295 = CARTESIAN_POINT ( 'NONE',  ( 43.01140435219951286, 101.0344580088725621, 29.21067981925356705 ) ) ;
#12296 = CARTESIAN_POINT ( 'NONE',  ( 40.27526882409969744, 108.5651871740939924, 37.97664729208901235 ) ) ;
#12297 = ORIENTED_EDGE ( 'NONE', *, *, #12053, .T. ) ;
#12298 = CARTESIAN_POINT ( 'NONE',  ( 48.01140435219951996, 157.1344580088725422, 35.83527830041809636 ) ) ;
#12299 = B_SPLINE_CURVE_WITH_KNOTS ( 'NONE', 1,
 ( #13278, #4445 ),
 .UNSPECIFIED., .F., .F.,
 ( 2, 2 ),
 ( 0.000000000000000000, 1.000000000000000000 ),
 .UNSPECIFIED. ) ;
#12300 = CARTESIAN_POINT ( 'NONE',  ( 19.03178791447554374, 95.58698510358173905, 9.200771007679692914 ) ) ;
#12301 = CARTESIAN_POINT ( 'NONE',  ( 21.71662816054514167, 101.4213758857254675, 8.370706496969875232 ) ) ;
#12302 = CARTESIAN_POINT ( 'NONE',  ( -141.4692556286852891, -169.1391397928654214, 52.90620854394536821 ) ) ;
#12303 = MECHANICAL_DESIGN_GEOMETRIC_PRESENTATION_REPRESENTATION (  '', ( #1042 ), #3867 ) ;
#12304 = ADVANCED_FACE ( 'NONE', ( #480 ), #6890, .T. ) ;
#12305 = CARTESIAN_POINT ( 'NONE',  ( 45.74753988029934249, 76.42977050742730682, 37.97664729208901235 ) ) ;
#12306 = EDGE_CURVE ( 'NONE', #13533, #7143, #20657, .T. ) ;
#12307 = VERTEX_POINT ( 'NONE', #15373 ) ;
#12308 = CARTESIAN_POINT ( 'NONE',  ( 38.01140435219951996, 62.93445800887258201, 35.83527830041810347 ) ) ;
#12309 = DIRECTION ( 'NONE',  ( -0.000000000000000000, -1.000000000000000000, -0.000000000000000000 ) ) ;
#12310 = EDGE_CURVE ( 'NONE', #495, #20113, #20792, .T. ) ;
#12311 = CARTESIAN_POINT ( 'NONE',  ( 46.10157429594899270, 128.6604996726487400, 29.95742577749337343 ) ) ;
#12313 = CARTESIAN_POINT ( 'NONE',  ( 11.38715737009742668, 107.0096734253407362, 2.652989958896663225 ) ) ;
#12312 = CARTESIAN_POINT ( 'NONE',  ( 38.58424406990784661, 77.96518717409396970, 32.77220824515698183 ) ) ;
#12314 = CARTESIAN_POINT ( 'NONE',  ( -154.3824083646099439, -182.4938272943107336, 40.69124936498395328 ) ) ;
#12315 = CARTESIAN_POINT ( 'NONE',  ( 39.92123440845005433, 116.3344580088725735, 29.95742577749336988 ) ) ;
#12316 = CARTESIAN_POINT ( 'NONE',  ( -157.6495955161842062, -187.1130981290893089, 58.16351966513671812 ) ) ;
#12317 = CARTESIAN_POINT ( 'NONE',  ( 38.96631938032478359, 81.08445800887258770, 37.14960608071593384 ) ) ;
#12318 = AXIS2_PLACEMENT_3D ( 'NONE', #16310, #7954, #4739 ) ;
#12319 = DIRECTION ( 'NONE',  ( 0.000000000000000000, -0.000000000000000000, -1.000000000000000000 ) ) ;
#12320 = FACE_OUTER_BOUND ( 'NONE', #13799, .T. ) ;
#12321 = CARTESIAN_POINT ( 'NONE',  ( 38.58424406990784661, 138.5297705074273154, 35.64915139335016647 ) ) ;
#12322 = CARTESIAN_POINT ( 'NONE',  ( 47.43856463449118621, 106.8797705074273239, 34.21067981925357060 ) ) ;
#12323 = CARTESIAN_POINT ( 'NONE',  ( 31.47436479266152531, 87.67613096727390598, 14.72005176623422606 ) ) ;
#12324 = CARTESIAN_POINT ( 'NONE',  ( 46.59305225739526435, 139.3151871740940067, 36.81289934271958941 ) ) ;
#12325 = CARTESIAN_POINT ( 'NONE',  ( 46.10157429594899270, 67.73445800887256496, 29.95742577749336988 ) ) ;
#12326 = CARTESIAN_POINT ( 'NONE',  ( -143.8425227516148084, -165.3584106276440480, 44.11586579668791330 ) ) ;
#12327 = CARTESIAN_POINT ( 'NONE',  ( -151.4692556286853176, -163.7391397928654726, 59.65701158161632378 ) ) ;
#12328 = CARTESIAN_POINT ( 'NONE',  ( 41.46631938032478359, 136.3104996726487457, 38.96596240072933170 ) ) ;
#12329 = CARTESIAN_POINT ( 'NONE',  ( 55.65775942066846937, 145.2030105016711445, 10.43785198868815023 ) ) ;
#12330 = PLANE ( 'NONE',  #10243 ) ;
#12331 = CARTESIAN_POINT ( 'NONE',  ( 43.01140435219951286, 113.3651871740939754, 29.55568802177586463 ) ) ;
#12332 = EDGE_CURVE ( 'NONE', #5667, #10538, #15477, .T. ) ;
#12333 = ORIENTED_EDGE ( 'NONE', *, *, #21480, .T. ) ;
#12334 = AXIS2_PLACEMENT_3D ( 'NONE', #10799, #976, #20720 ) ;
#12335 = CARTESIAN_POINT ( 'NONE',  ( -151.4692556286852891, -178.7391397928654726, 59.65701158161631668 ) ) ;
#12336 = VERTEX_POINT ( 'NONE', #17333 ) ;
#12337 = CARTESIAN_POINT ( 'NONE',  ( 44.55648932407425633, 96.68445800887258201, 38.96596240072933170 ) ) ;
#12338 = CARTESIAN_POINT ( 'NONE',  ( 44.37947211624943833, 146.4797705074273324, 30.00020018409699318 ) ) ;
#12339 = CARTESIAN_POINT ( 'NONE',  ( 43.01140435219951286, 158.9604996726487514, 28.95336869806222779 ) ) ;
#12341 = CARTESIAN_POINT ( 'NONE',  ( 28.97945247615869846, 95.53788343559241980, -5.005900276531492388 ) ) ;
#12340 = CARTESIAN_POINT ( 'NONE',  ( 44.37947211624943833, 121.0151871740940095, 38.42115945441014446 ) ) ;
#12342 = CARTESIAN_POINT ( 'NONE',  ( 39.92123440845004723, 76.16049967264872578, 38.46393386101376421 ) ) ;
#12344 = CARTESIAN_POINT ( 'NONE',  ( 126.8576204525573274, -126.9891397928655010, 67.64809332337412684 ) ) ;
#12343 = CARTESIAN_POINT ( 'NONE',  ( 42.21948215057684450, 108.4575765865522925, 39.21067981925356349 ) ) ;
#12345 = CARTESIAN_POINT ( 'NONE',  ( 47.05648932407426344, 82.58445800887258770, 31.27175355779120025 ) ) ;
#12346 = CARTESIAN_POINT ( 'NONE',  ( 43.01140435219957681, 71.03445800887256212, 29.21067981925356705 ) ) ;
#12347 = CARTESIAN_POINT ( 'NONE',  ( 46.06149648801706320, 95.09233299183981103, 38.18604851697274682 ) ) ;
#12348 =( BOUNDED_CURVE ( )  B_SPLINE_CURVE ( 1, ( #4435, #2791 ),
 .UNSPECIFIED., .F., .F. ) 
 B_SPLINE_CURVE_WITH_KNOTS ( ( 2, 2 ),
 ( 0.000000000000000000, 1.000000000000000000 ),
 .UNSPECIFIED. ) 
 CURVE ( )  GEOMETRIC_REPRESENTATION_ITEM ( )  RATIONAL_B_SPLINE_CURVE ( ( 0.9782074146920120006, 0.9782074146920120006 ) ) 
 REPRESENTATION_ITEM ( '' )  );
#12349 = CARTESIAN_POINT ( 'NONE',  ( 47.43856463449117200, 70.76518717409399528, 32.77220824515698183 ) ) ;
#12350 = CARTESIAN_POINT ( 'NONE',  ( 84.42064422693164261, 282.0082918409407284, -4.000000000000003553 ) ) ;
#12351 = CARTESIAN_POINT ( 'NONE',  ( -151.4692556286852891, -184.1438272943107108, 59.56931450028537967 ) ) ;
#12352 = CARTESIAN_POINT ( 'NONE',  ( 43.01140435219951996, 119.9070776186055838, -35.00000000000000000 ) ) ;
#12353 = VERTEX_POINT ( 'NONE', #20869 ) ;
#12354 = CARTESIAN_POINT ( 'NONE',  ( -154.3824083646099439, -178.5584106276440366, 58.62277379824867296 ) ) ;
#12355 = CARTESIAN_POINT ( 'NONE',  ( 47.52490801233957995, 85.89149910694642642, 6.191896081848653921 ) ) ;
#12356 = ORIENTED_EDGE ( 'NONE', *, *, #17652, .F. ) ;
#12357 = CARTESIAN_POINT ( 'NONE',  ( 47.43856463449117200, 145.7651871740939953, 32.77220824515698183 ) ) ;
#12358 = FACE_BOUND ( 'NONE', #12466, .T. ) ;
#12359 = CARTESIAN_POINT ( 'NONE',  ( 43.01140435219951286, 109.1297705074273239, 38.86567161673127657 ) ) ;
#12360 = ORIENTED_EDGE ( 'NONE', *, *, #1349, .T. ) ;
#12361 = VERTEX_POINT ( 'NONE', #12702 ) ;
#12362 = CARTESIAN_POINT ( 'NONE',  ( 70.85748824340309682, 124.3570181999574515, -1.510321027129504889 ) ) ;
#12363 = VERTEX_POINT ( 'NONE', #4320 ) ;
#12364 = CARTESIAN_POINT ( 'NONE',  ( 41.64333658814960870, 110.7797705074273154, 30.00020018409699318 ) ) ;
#12365 = DIRECTION ( 'NONE',  ( 0.000000000000000000, 0.000000000000000000, 1.000000000000000000 ) ) ;
#12366 = CARTESIAN_POINT ( 'NONE',  ( 39.42975644700377558, 149.8151871740940067, 31.60846029578754468 ) ) ;
#12367 = CARTESIAN_POINT ( 'NONE',  ( 47.05648932407426344, 103.9104996726487400, 37.14960608071593384 ) ) ;
#12368 = CARTESIAN_POINT ( 'NONE',  ( 73.32203938827501588, 103.9946350594383517, -0.8753108214479579097 ) ) ;
#12369 = CARTESIAN_POINT ( 'NONE',  ( -151.4692556286852891, -180.8130981290893260, 59.65701158161631668 ) ) ;
#12370 = CARTESIAN_POINT ( 'NONE',  ( -148.3790856849358306, -168.3891397928654499, 40.14644641866477315 ) ) ;
#12371 = LINE ( 'NONE', #17436, #4855 ) ;
#12372 = UNCERTAINTY_MEASURE_WITH_UNIT (LENGTH_MEASURE( 1.000000000000000082E-05 ), #8827, 'distance_accuracy_value', 'NONE');
#12373 = ADVANCED_FACE ( 'NONE', ( #12486 ), #19423, .T. ) ;
#12374 = CARTESIAN_POINT ( 'NONE',  ( 43.01140435219951286, 143.0344580088726048, 29.21067981925356705 ) ) ;
#12375 = VECTOR ( 'NONE', #270, 1000.000000000000000 ) ;
#12376 = APPLICATION_CONTEXT ( 'automotive_design' ) ;
#12377 = CARTESIAN_POINT ( 'NONE',  ( -157.6495955161842062, -164.0130981290892578, 41.15050349809589392 ) ) ;
#12378 = VECTOR ( 'NONE', #9039, 1000.000000000000000 ) ;
#12379 = VERTEX_POINT ( 'NONE', #21093 ) ;
#12380 = CARTESIAN_POINT ( 'NONE',  ( 44.37947211624943833, 88.27977050742731535, 38.42115945441014446 ) ) ;
#12381 = CARTESIAN_POINT ( 'NONE',  ( -143.8425227516148084, -165.6938272943107222, 55.19815736654470584 ) ) ;
#12382 = CARTESIAN_POINT ( 'NONE',  ( 41.64333658814960870, 68.51518717409399528, 30.00020018409699318 ) ) ;
#12383 = CARTESIAN_POINT ( 'NONE',  ( 20.91437931538276374, 145.9617080342048894, -10.94665030085253044 ) ) ;
#12384 = CARTESIAN_POINT ( 'NONE',  ( -160.8964159109769696, -194.0084106276440252, 52.72008163687743121 ) ) ;
#12385 = VECTOR ( 'NONE', #1616, 1000.000000000000000 ) ;
#12386 = EDGE_LOOP ( 'NONE', ( #18338, #12705, #3674, #16726, #10238, #9940, #18221, #1807, #6721, #7252 ) ) ;
#12387 = CARTESIAN_POINT ( 'NONE',  ( 39.92123440845005433, 69.23445800887257917, 38.46393386101375711 ) ) ;
#12388 = CARTESIAN_POINT ( 'NONE',  ( 136.0032066456581390, 182.5367998656340944, 14.00000000000001776 ) ) ;
#12389 = CARTESIAN_POINT ( 'NONE',  ( 45.74753988029934249, 131.3297705074273267, 30.44471234641812174 ) ) ;
#12390 = CARTESIAN_POINT ( 'NONE',  ( 19.47480796662762970, 104.5210170170265229, 9.517959287447121497 ) ) ;
#12391 = ORIENTED_EDGE ( 'NONE', *, *, #9740, .F. ) ;
#12392 = DIRECTION ( 'NONE',  ( -0.000000000000000000, -0.000000000000000000, 1.000000000000000000 ) ) ;
#12393 = EDGE_LOOP ( 'NONE', ( #9636, #11246, #14393, #12582 ) ) ;
#12394 = CARTESIAN_POINT ( 'NONE',  ( 38.58424406990784661, 138.5297705074273154, 35.64915139335016647 ) ) ;
#12395 = EDGE_CURVE ( 'NONE', #12901, #19172, #1329, .T. ) ;
#12396 = AXIS2_PLACEMENT_3D ( 'NONE', #19385, #4495, #14633 ) ;
#12397 = CARTESIAN_POINT ( 'NONE',  ( 41.64333658814960870, 92.77977050742731535, 30.00020018409699318 ) ) ;
#12398 = CIRCLE ( 'NONE', #20858, 14.42424326798555434 ) ;
#12399 = DIRECTION ( 'NONE',  ( 0.000000000000000000, 1.000000000000000000, 0.000000000000000000 ) ) ;
#12400 = CARTESIAN_POINT ( 'NONE',  ( 45.74753988029933538, 101.0651871740939924, 30.44471234641811819 ) ) ;
#12401 = CARTESIAN_POINT ( 'NONE',  ( 42.21948215057684450, 66.03738109496899256, 29.21067981925356705 ) ) ;
#12402 = CARTESIAN_POINT ( 'NONE',  ( 136.2275274985377678, 181.9605282764600815, 22.92609503421871864 ) ) ;
#12403 = CARTESIAN_POINT ( 'NONE',  ( -141.4692556286852891, -156.2130981290893317, 52.90620854394536821 ) ) ;
#12404 = DIRECTION ( 'NONE',  ( 1.000000000000000000, 0.000000000000000000, 0.000000000000000000 ) ) ;
#12405 = CARTESIAN_POINT ( 'NONE',  ( -151.4692556286852891, -196.9891397928655010, 39.65701158161630246 ) ) ;
#12406 = CARTESIAN_POINT ( 'NONE',  ( 38.96631938032478359, 134.4844580088725934, 31.27175355779120025 ) ) ;
#12407 = CARTESIAN_POINT ( 'NONE',  ( 40.27526882409969033, 110.9297705074272926, 30.44471234641811819 ) ) ;
#12408 = CARTESIAN_POINT ( 'NONE',  ( 34.25380259335813093, 93.01594701623474748, 13.77127495354717190 ) ) ;
#12409 = CARTESIAN_POINT ( 'NONE',  ( -143.8425227516148084, -195.0938272943107279, 44.11586579668791330 ) ) ;
#12410 = CARTESIAN_POINT ( 'NONE',  ( 43.01140435219951286, 107.3651871740940038, 29.55568802177586107 ) ) ;
#12411 = CARTESIAN_POINT ( 'NONE',  ( 137.5268905834513191, 193.0332408774651185, 14.00000000000001776 ) ) ;
#12412 = ORIENTED_EDGE ( 'NONE', *, *, #601, .T. ) ;
#12413 = CARTESIAN_POINT ( 'NONE',  ( 43.01140435219951286, 77.03445800887257633, 29.21067981925356705 ) ) ;
#12414 = EDGE_CURVE ( 'NONE', #1800, #12361, #21510, .T. ) ;
#12415 = CARTESIAN_POINT ( 'NONE',  ( 27.91901995959459271, 89.26896823883201648, 8.843372880480211862 ) ) ;
#12416 = CARTESIAN_POINT ( 'NONE',  ( 71.07552608251525328, 117.1481954606975791, 12.77539325861266484 ) ) ;
#12417 = ADVANCED_BREP_SHAPE_REPRESENTATION ( '', ( #21529, #12657 ), #7037 ) ;
#12418 = CARTESIAN_POINT ( 'NONE',  ( 43.01140435219953417, 138.5344580088726048, 39.21067981925356349 ) ) ;
#12419 = CARTESIAN_POINT ( 'NONE',  ( 41.64333658814960870, 80.77977050742732956, 30.00020018409699318 ) ) ;
#12420 = ORIENTED_EDGE ( 'NONE', *, *, #12044, .T. ) ;
#12421 = ORIENTED_EDGE ( 'NONE', *, *, #929, .F. ) ;
#12422 = PRODUCT_DEFINITION ( 'UNKNOWN', '', #3173, #8411 ) ;
#12423 = CARTESIAN_POINT ( 'NONE',  ( -149.8854112254399240, -172.6622583705452314, 59.65701158161632378 ) ) ;
#12425 = ADVANCED_FACE ( 'NONE', ( #21502 ), #7327, .F. ) ;
#12424 = CARTESIAN_POINT ( 'NONE',  ( 44.55648932407425633, 118.6104996726487570, 38.96596240072933170 ) ) ;
#12427 = CARTESIAN_POINT ( 'NONE',  ( 51.97100187899584967, 152.8641821122263309, -1.870631353872792335 ) ) ;
#12426 = CARTESIAN_POINT ( 'NONE',  ( 40.27526882409969033, 77.66518717409400097, 30.44471234641811819 ) ) ;
#12428 = CARTESIAN_POINT ( 'NONE',  ( -145.6429501568359797, -170.9438272943107222, 41.63779006702063867 ) ) ;
#12429 = CARTESIAN_POINT ( 'NONE',  ( 62.84376099716368458, 92.00366499689042143, 13.64888190966157566 ) ) ;
#12430 = CARTESIAN_POINT ( 'NONE',  ( -141.4692556286852891, -186.0630981290892976, 49.65701158161630957 ) ) ;
#12431 = CARTESIAN_POINT ( 'NONE',  ( 38.96631938032478359, 80.48445800887257917, 31.27175355779120025 ) ) ;
#12432 = LINE ( 'NONE', #7808, #15301 ) ;
#12433 = CARTESIAN_POINT ( 'NONE',  ( -151.4692556286852607, -162.2391397928654442, 39.65701158161629536 ) ) ;
#12434 = CARTESIAN_POINT ( 'NONE',  ( 45.74753988029933538, 142.4297705074273495, 37.97664729208901946 ) ) ;
#12435 = EDGE_CURVE ( 'NONE', #10777, #1337, #2761, .T. ) ;
#12436 = CARTESIAN_POINT ( 'NONE',  ( 54.37136329154349568, 152.2862128563062072, 3.215626235130811583 ) ) ;
#12437 = CARTESIAN_POINT ( 'NONE',  ( 38.58424406990785371, 135.2651871740939953, 35.64915139335015937 ) ) ;
#12438 = CARTESIAN_POINT ( 'NONE',  ( 43.01140435219957681, 94.46049967264876557, 39.21067981925356349 ) ) ;
#12439 = CARTESIAN_POINT ( 'NONE',  ( -151.4692556286852891, -166.4084106276440593, 59.56931450028537256 ) ) ;
#12440 = CARTESIAN_POINT ( 'NONE',  ( 41.64333658814960870, 59.77977050742731535, 30.00020018409699318 ) ) ;
#12441 = CARTESIAN_POINT ( 'NONE',  ( 43.80332655382220253, 91.95757658655229250, 29.21067981925356705 ) ) ;
#12442 = CARTESIAN_POINT ( 'NONE',  ( 24.99951789580824268, 141.7104366081036346, 16.15213770299339657 ) ) ;
#12443 = DIRECTION ( 'NONE',  ( -1.000000000000000000, 0.000000000000000000, 0.000000000000000000 ) ) ;
#12444 = CARTESIAN_POINT ( 'NONE',  ( 39.42975644700377558, 119.8151871740940067, 31.60846029578754468 ) ) ;
#12445 = ORIENTED_EDGE ( 'NONE', *, *, #15641, .F. ) ;
#12446 = CARTESIAN_POINT ( 'NONE',  ( -154.5594255724347761, -161.1630981290892919, 40.14644641866476604 ) ) ;
#12447 = ORIENTED_EDGE ( 'NONE', *, *, #2945, .T. ) ;
#12448 = CARTESIAN_POINT ( 'NONE',  ( 46.10157429594899270, 87.83445800887255928, 38.46393386101376421 ) ) ;
#12449 = CARTESIAN_POINT ( 'NONE',  ( 47.43856463449117911, 148.7297705074273324, 35.64915139335015937 ) ) ;
#12450 = EDGE_CURVE ( 'NONE', #9101, #20743, #12371, .T. ) ;
#12451 = CARTESIAN_POINT ( 'NONE',  ( 38.01140435219952707, 150.7104996726487514, 34.21067981925357060 ) ) ;
#12453 = CARTESIAN_POINT ( 'NONE',  ( 54.97053026609068382, 94.45704024927961484, -6.077358488390353308 ) ) ;
#12452 = CARTESIAN_POINT ( 'NONE',  ( 46.59305225739526435, 106.9151871740940152, 31.60846029578754468 ) ) ;
#12454 = CARTESIAN_POINT ( 'NONE',  ( 41.46631938032478359, 72.11049967264874283, 29.45539723777780239 ) ) ;
#12456 = CARTESIAN_POINT ( 'NONE',  ( -154.5594255724347761, -156.9630981290893317, 59.16757674456785310 ) ) ;
#12455 = PLANE ( 'NONE',  #17489 ) ;
#12457 = CARTESIAN_POINT ( 'NONE',  ( -205.5014940257113665, 559.0624978195118047, 0.000000000000000000 ) ) ;
#12458 = LINE ( 'NONE', #14433, #4444 ) ;
#12459 = CARTESIAN_POINT ( 'NONE',  ( 46.59305225739526435, 67.31518717409400665, 36.81289934271958941 ) ) ;
#12460 = CARTESIAN_POINT ( 'NONE',  ( 38.01140435219952707, 63.56049967264873146, 32.58608133808903773 ) ) ;
#12461 = CARTESIAN_POINT ( 'NONE',  ( -148.5561028927606344, -179.7938272943107449, 40.69124936498395328 ) ) ;
#12462 = CARTESIAN_POINT ( 'NONE',  ( -151.4692556286852891, -190.4084106276440309, 59.56931450028537256 ) ) ;
#12463 = ORIENTED_EDGE ( 'NONE', *, *, #2025, .T. ) ;
#12464 = CARTESIAN_POINT ( 'NONE',  ( -157.2955611005346270, -181.7084106276440423, 57.67623309621198047 ) ) ;
#12465 = CARTESIAN_POINT ( 'NONE',  ( 67.29571637068438861, 144.1510613573267108, 10.71565575886252297 ) ) ;
#12466 = EDGE_LOOP ( 'NONE', ( #3240, #14980 ) ) ;
#12467 = CARTESIAN_POINT ( 'NONE',  ( 46.59305225739526435, 142.3151871740940067, 36.81289934271958941 ) ) ;
#12468 = EDGE_CURVE ( 'NONE', #4975, #5215, #5533, .T. ) ;
#12469 = CARTESIAN_POINT ( 'NONE',  ( 45.74753988029934249, 109.4297705074273352, 37.97664729208901235 ) ) ;
#12470 = ORIENTED_EDGE ( 'NONE', *, *, #11114, .T. ) ;
#12471 = ORIENTED_EDGE ( 'NONE', *, *, #18144, .T. ) ;
#12472 = CARTESIAN_POINT ( 'NONE',  ( 14.88799800344823154, 117.8296896831652560, 9.085076399755989129 ) ) ;
#12473 = ORIENTED_EDGE ( 'NONE', *, *, #12699, .F. ) ;
#12474 = CARTESIAN_POINT ( 'NONE',  ( 48.01140435219951996, 115.4344580088725678, 32.58608133808903773 ) ) ;
#12475 = CIRCLE ( 'NONE', #11766, 10.00000000000000888 ) ;
#12476 = DIRECTION ( 'NONE',  ( 1.000000000000000000, -0.000000000000000000, -1.140132994654635861E-16 ) ) ;
#12477 = EDGE_CURVE ( 'NONE', #4439, #14006, #1347, .T. ) ;
#12478 = EDGE_CURVE ( 'NONE', #21052, #17748, #3197, .T. ) ;
#12479 = CARTESIAN_POINT ( 'NONE',  ( 38.58424406990784661, 81.22977050742731819, 32.77220824515698183 ) ) ;
#12480 = CARTESIAN_POINT ( 'NONE',  ( 45.74753988029933538, 133.1651871740940010, 37.97664729208901946 ) ) ;
#12481 =( BOUNDED_CURVE ( )  B_SPLINE_CURVE ( 2, ( #11972, #17357, #2262, #8999, #75, #6813, #18701, #17141, #13519, #20252, #3607, #294, #10330 ),
 .UNSPECIFIED., .F., .F. ) 
 B_SPLINE_CURVE_WITH_KNOTS ( ( 3, 2, 2, 2, 2, 2, 3 ),
 ( 0.4821428571428571508, 0.4857142857142857095, 0.4928571428571428825, 0.5000000000000000000, 0.5071428571428571175, 0.5142857142857142350, 0.5178571428571429047 ),
 .UNSPECIFIED. ) 
 CURVE ( )  GEOMETRIC_REPRESENTATION_ITEM ( )  RATIONAL_B_SPLINE_CURVE ( ( 0.9755282581475768211, 0.9755282581475768211, 1.000000000000000000, 0.9510565162951535312, 1.000000000000000000, 0.9510565162951535312, 1.000000000000000000, 0.9510565162951535312, 1.000000000000000000, 0.9510565162951535312, 1.000000000000000000, 0.9755282581475763770, 0.9755282581475768211 ) ) 
 REPRESENTATION_ITEM ( '' )  );
#12482 = CARTESIAN_POINT ( 'NONE',  ( 47.05648932407426344, 100.9104996726487400, 37.14960608071593384 ) ) ;
#12483 = CARTESIAN_POINT ( 'NONE',  ( 18.20936163119166196, 143.5026679720446907, 2.934308097026923967 ) ) ;
#12484 = CARTESIAN_POINT ( 'NONE',  ( 136.0836978799983967, 182.3207987053756938, 19.41518736053559024 ) ) ;
#12485 = CARTESIAN_POINT ( 'NONE',  ( -154.5594255724347761, -172.8891397928654783, 59.16757674456785310 ) ) ;
#12486 = FACE_OUTER_BOUND ( 'NONE', #978, .T. ) ;
#12487 = CARTESIAN_POINT ( 'NONE',  ( 39.92123440845005433, 144.2344580088725934, 38.46393386101375711 ) ) ;
#12488 = CARTESIAN_POINT ( 'NONE',  ( -153.0531000319307111, -164.2362167067690564, 39.65701158161631668 ) ) ;
#12489 = ORIENTED_EDGE ( 'NONE', *, *, #21126, .F. ) ;
#12490 = CARTESIAN_POINT ( 'NONE',  ( 45.74753988029933538, 86.32977050742729830, 30.44471234641811819 ) ) ;
#12491 = CARTESIAN_POINT ( 'NONE',  ( -159.0959885057557983, -166.5938272943107563, 55.19815736654470584 ) ) ;
#12492 = CARTESIAN_POINT ( 'NONE',  ( 40.27526882409969744, 72.56518717409399244, 37.97664729208901235 ) ) ;
#12493 = CARTESIAN_POINT ( 'NONE',  ( 69.27296957579615366, 97.94681810169329594, -0.6368323762655749842 ) ) ;
#12494 = ADVANCED_FACE ( 'NONE', ( #108 ), #6623, .T. ) ;
#12495 = CARTESIAN_POINT ( 'NONE',  ( -148.5561028927606344, -192.0584106276440650, 40.69124936498395328 ) ) ;
#12496 = ORIENTED_EDGE ( 'NONE', *, *, #18992, .T. ) ;
#12497 = CARTESIAN_POINT ( 'NONE',  ( 43.80332655382220253, 84.61133943119283174, 39.21067981925355639 ) ) ;
#12498 = CARTESIAN_POINT ( 'NONE',  ( -101.1064508287285832, 10.96617311717548660, -19.99999999999997868 ) ) ;
#12499 = CARTESIAN_POINT ( 'NONE',  ( 45.74753988029934249, 136.4297705074273210, 37.97664729208901235 ) ) ;
#12500 = CARTESIAN_POINT ( 'NONE',  ( 19.07518309319397432, 143.9976739860571229, -17.03742665657317801 ) ) ;
#12501 = EDGE_LOOP ( 'NONE', ( #7844, #9339, #6990, #17562 ) ) ;
#12502 = FACE_OUTER_BOUND ( 'NONE', #13290, .T. ) ;
#12503 = ORIENTED_EDGE ( 'NONE', *, *, #8140, .T. ) ;
#12504 = CARTESIAN_POINT ( 'NONE',  ( 44.37947211624943833, 130.2797705074273154, 38.42115945441014446 ) ) ;
#12505 = EDGE_CURVE ( 'NONE', #10720, #3622, #18295, .T. ) ;
#12506 = CARTESIAN_POINT ( 'NONE',  ( 48.01140435219951996, 110.0604996726487315, 35.83527830041809636 ) ) ;
#12507 = CYLINDRICAL_SURFACE ( 'NONE', #4922, 10.00000000000000888 ) ;
#12508 = CARTESIAN_POINT ( 'NONE',  ( 43.01140435219951286, 98.96049967264873715, 29.21067981925356705 ) ) ;
#12509 = CARTESIAN_POINT ( 'NONE',  ( 163.1026836591718734, 192.4288937294299160, 14.00000000000001776 ) ) ;
#12510 = SURFACE_STYLE_FILL_AREA ( #12177 ) ;
#12511 = CARTESIAN_POINT ( 'NONE',  ( 41.64333658814960870, 99.71518717409399812, 38.42115945441014446 ) ) ;
#12512 = CARTESIAN_POINT ( 'NONE',  ( 43.01140435219951996, 10.71049967264875491, 39.21067981925356349 ) ) ;
#12513 = CARTESIAN_POINT ( 'NONE',  ( 136.0032066456581390, 182.5367998656340944, 24.47866928663567521 ) ) ;
#12514 = CARTESIAN_POINT ( 'NONE',  ( -154.5594255724347761, -155.1630981290892919, 40.14644641866476604 ) ) ;
#12515 = APPLICATION_PROTOCOL_DEFINITION ( 'draft international standard', 'automotive_design', 1998, #8307 ) ;
#12516 = VECTOR ( 'NONE', #13391, 1000.000000000000000 ) ;
#12517 = CARTESIAN_POINT ( 'NONE',  ( 43.80332655382220253, 70.53738109496900677, 39.21067981925355639 ) ) ;
#12518 = CARTESIAN_POINT ( 'NONE',  ( 39.92123440845004723, 131.3344580088725593, 29.95742577749337343 ) ) ;
#12519 = CARTESIAN_POINT ( 'NONE',  ( 38.58424406990784661, 117.2297705074273040, 32.77220824515698183 ) ) ;
#12520 = CARTESIAN_POINT ( 'NONE',  ( 70.90273821555796019, 124.5833669296562931, 4.485287862780372947 ) ) ;
#12521 = CARTESIAN_POINT ( 'NONE',  ( 45.74753988029934249, 97.16518717409398675, 37.97664729208901235 ) ) ;
#12522 = CARTESIAN_POINT ( 'NONE',  ( 151.4773229304660731, 84.89323405393692212, 4.000000000000021316 ) ) ;
#12523 = ORIENTED_EDGE ( 'NONE', *, *, #8819, .F. ) ;
#12524 = CARTESIAN_POINT ( 'NONE',  ( 44.55648932407425633, 157.8844580088725706, 29.45539723777780239 ) ) ;
#12525 = CARTESIAN_POINT ( 'NONE',  ( 69.71972837475884432, 98.49221204361529658, -7.660766391518695428 ) ) ;
#12526 = CARTESIAN_POINT ( 'NONE',  ( 66.10898071834657230, 103.7292514542787245, 6.347102411281516865 ) ) ;
#12527 = CARTESIAN_POINT ( 'NONE',  ( 43.01140435219951996, 10.71049967264875491, 34.21067981925357060 ) ) ;
#12528 = AXIS2_PLACEMENT_3D ( 'NONE', #9687, #18490, #21806 ) ;
#12529 = CARTESIAN_POINT ( 'NONE',  ( 45.74753988029934249, 77.32977050742729830, 30.44471234641812174 ) ) ;
#12530 = EDGE_LOOP ( 'NONE', ( #14715, #11407 ) ) ;
#12531 = ORIENTED_EDGE ( 'NONE', *, *, #19202, .T. ) ;
#12532 = CARTESIAN_POINT ( 'NONE',  ( 43.01140435219951996, 10.71049967264875491, 29.21067981925357060 ) ) ;
#12533 = CARTESIAN_POINT ( 'NONE',  ( 47.05648932407426344, 124.9104996726487542, 37.14960608071593384 ) ) ;
#12535 = CARTESIAN_POINT ( 'NONE',  ( 21.10625685842435928, 146.1099207202125854, -2.942173209646314014 ) ) ;
#12534 = CARTESIAN_POINT ( 'NONE',  ( 47.43856463449117200, 76.46518717409401233, 35.64915139335016647 ) ) ;
#12536 = CARTESIAN_POINT ( 'NONE',  ( -151.4692556286852891, -172.1438272943107393, 59.56931450028537256 ) ) ;
#12537 = CARTESIAN_POINT ( 'NONE',  ( 75.59501567365037999, 109.4093883240155378, 12.93430809701916750 ) ) ;
#12538 = CARTESIAN_POINT ( 'NONE',  ( -159.5594255724347761, -184.8630981290893089, 43.77915905869157598 ) ) ;
#12539 =( NAMED_UNIT ( * ) SI_UNIT ( $, .STERADIAN. ) SOLID_ANGLE_UNIT ( ) );
#12540 = CARTESIAN_POINT ( 'NONE',  ( 43.01140435219951286, 88.46049967264873715, 39.21067981925356349 ) ) ;
#12541 = DIRECTION ( 'NONE',  ( -0.09993390301907582873, 0.9949940778855791423, 0.000000000000000000 ) ) ;
#12542 = CARTESIAN_POINT ( 'NONE',  ( 39.42975644700377558, 138.0797705074273267, 31.60846029578754468 ) ) ;
#12543 = CARTESIAN_POINT ( 'NONE',  ( 23.80922038702690102, 91.46939207759763235, 0.001460074241615882690 ) ) ;
#12544 = CARTESIAN_POINT ( 'NONE',  ( 38.58424406990785371, 129.2651871740940237, 35.64915139335015937 ) ) ;
#12545 = CARTESIAN_POINT ( 'NONE',  ( 47.05648932407426344, 137.5104996726487627, 31.27175355779120025 ) ) ;
#12546 = CARTESIAN_POINT ( 'NONE',  ( -142.0420953463935803, -162.5084106276440536, 46.59394152635518083 ) ) ;
#12547 = CARTESIAN_POINT ( 'NONE',  ( 162.0641828542163125, 116.7231784796025948, 4.000000000000021316 ) ) ;
#12548 = VECTOR ( 'NONE', #18670, 1000.000000000000000 ) ;
#12549 = EDGE_CURVE ( 'NONE', #4204, #11358, #2063, .T. ) ;
#12550 = CARTESIAN_POINT ( 'NONE',  ( 44.55648932407425633, 91.88445800887258486, 29.45539723777780239 ) ) ;
#12551 = CARTESIAN_POINT ( 'NONE',  ( 64.86034851325717909, 101.9512479430583625, 5.437578391810254708 ) ) ;
#12552 = CARTESIAN_POINT ( 'NONE',  ( 141.4773229304660447, 84.89323405393692212, 14.00000000000001776 ) ) ;
#12553 = CARTESIAN_POINT ( 'NONE',  ( 38.58424406990784661, 107.9651871740939839, 32.77220824515698183 ) ) ;
#12554 = ORIENTED_EDGE ( 'NONE', *, *, #3935, .T. ) ;
#12555 = DIRECTION ( 'NONE',  ( -0.3450121214752274179, 0.9385982292947088190, 0.000000000000000000 ) ) ;
#12556 = EDGE_LOOP ( 'NONE', ( #14041, #20646, #3836, #16667 ) ) ;
#12557 = CARTESIAN_POINT ( 'NONE',  ( 47.05648932407426344, 94.58445800887257349, 31.27175355779120025 ) ) ;
#12558 = AXIS2_PLACEMENT_3D ( 'NONE', #11389, #452, #9976 ) ;
#12559 = CARTESIAN_POINT ( 'NONE',  ( 44.37947211624943833, 152.4797705074273324, 30.00020018409699318 ) ) ;
#12560 = CARTESIAN_POINT ( 'NONE',  ( 38.01140435219951996, 144.5604996726487173, 32.58608133808903773 ) ) ;
#12562 = CARTESIAN_POINT ( 'NONE',  ( 60.50179475597519740, 141.9260456451392827, -8.339099203377070779 ) ) ;
#12561 = CARTESIAN_POINT ( 'NONE',  ( 47.43856463449118621, 106.6151871740940038, 34.21067981925357060 ) ) ;
#12563 = LINE ( 'NONE', #2531, #605 ) ;
#12565 = DIRECTION ( 'NONE',  ( 0.000000000000000000, 0.000000000000000000, 1.000000000000000000 ) ) ;
#12564 = DIRECTION ( 'NONE',  ( 1.000000000000000000, 0.000000000000000000, 0.000000000000000000 ) ) ;
#12566 = PLANE ( 'NONE',  #8442 ) ;
#12567 = DIRECTION ( 'NONE',  ( 1.000000000000000000, 0.000000000000000000, 0.000000000000000000 ) ) ;
#12568 = LINE ( 'NONE', #7731, #13258 ) ;
#12569 = CARTESIAN_POINT ( 'NONE',  ( 39.42975644700377558, 65.81518717409400665, 31.60846029578754468 ) ) ;
#12570 = CARTESIAN_POINT ( 'NONE',  ( 61.61057083318216598, 91.16763906547615193, -7.303593892219363504 ) ) ;
#12571 = CARTESIAN_POINT ( 'NONE',  ( 43.80332655382220253, 103.5373810949689926, 39.21067981925355639 ) ) ;
#12572 = CARTESIAN_POINT ( 'NONE',  ( -157.2955611005346270, -169.4438272943107222, 57.67623309621198047 ) ) ;
#12573 = CARTESIAN_POINT ( 'NONE',  ( -151.4692556286852891, -196.9891397928655010, 49.65701158161630957 ) ) ;
#12574 = EDGE_LOOP ( 'NONE', ( #5299, #18215 ) ) ;
#12575 = CARTESIAN_POINT ( 'NONE',  ( -151.4692556286852891, -179.9084106276440593, 39.74470866294723947 ) ) ;
#12576 = AXIS2_PLACEMENT_3D ( 'NONE', #3924, #20358, #20681 ) ;
#12577 = CARTESIAN_POINT ( 'NONE',  ( 77.28446211531542076, 118.2294073780637262, 4.644197663618684579 ) ) ;
#12578 = DIRECTION ( 'NONE',  ( 0.000000000000000000, 0.000000000000000000, 1.000000000000000000 ) ) ;
#12579 = CARTESIAN_POINT ( 'NONE',  ( 38.58424406990784661, 143.9651871740940123, 32.77220824515698183 ) ) ;
#12580 = CARTESIAN_POINT ( 'NONE',  ( 47.43856463449117911, 157.4651871740939839, 35.64915139335015937 ) ) ;
#12581 = CARTESIAN_POINT ( 'NONE',  ( 40.27526882409969744, 93.82977050742731251, 37.97664729208901235 ) ) ;
#12582 = ORIENTED_EDGE ( 'NONE', *, *, #6177, .F. ) ;
#12583 = ORIENTED_EDGE ( 'NONE', *, *, #11250, .F. ) ;
#12584 = EDGE_CURVE ( 'NONE', #13613, #13351, #6840, .T. ) ;
#12585 = CARTESIAN_POINT ( 'NONE',  ( 62.59245796673033624, 99.61375035622579333, -0.4388640268946644718 ) ) ;
#12586 = ORIENTED_EDGE ( 'NONE', *, *, #8508, .T. ) ;
#12587 = EDGE_CURVE ( 'NONE', #11679, #2742, #20690, .T. ) ;
#12588 = CARTESIAN_POINT ( 'NONE',  ( 38.96631938032478359, 113.4844580088725792, 31.27175355779120025 ) ) ;
#12589 = AXIS2_PLACEMENT_3D ( 'NONE', #14144, #10308, #8440 ) ;
#12590 = CARTESIAN_POINT ( 'NONE',  ( 116.4417310231185780, -136.9891397928655010, 0.3429884183836981459 ) ) ;
#12591 = CARTESIAN_POINT ( 'NONE',  ( 46.59305225739526435, 73.57977050742732672, 36.81289934271958941 ) ) ;
#12592 = CARTESIAN_POINT ( 'NONE',  ( 40.27526882409969033, 138.5651871740939498, 37.97664729208901946 ) ) ;
#12593 = VECTOR ( 'NONE', #15078, 1000.000000000000000 ) ;
#12594 = CARTESIAN_POINT ( 'NONE',  ( 38.01140435219951996, 90.86049967264871441, 35.83527830041810347 ) ) ;
#12595 = CARTESIAN_POINT ( 'NONE',  ( 11.39584491653312526, 106.7788786240791978, 8.648593811254444930 ) ) ;
#12596 = CARTESIAN_POINT ( 'NONE',  ( 38.26722257261177873, 95.36101971774161257, 35.82300994916139558 ) ) ;
#12597 = CARTESIAN_POINT ( 'NONE',  ( -141.4692556286852891, -157.1391397928654783, 52.90620854394536821 ) ) ;
#12598 = CARTESIAN_POINT ( 'NONE',  ( 48.01140435219951996, 158.3604996726487286, 32.58608133808903773 ) ) ;
#12599 = CARTESIAN_POINT ( 'NONE',  ( 48.01140435219951996, 64.28445800887257633, 34.21067981925357060 ) ) ;
#12600 = ORIENTED_EDGE ( 'NONE', *, *, #10936, .T. ) ;
#12601 = CARTESIAN_POINT ( 'NONE',  ( 46.59305225739526435, 74.17977050742732104, 31.60846029578754468 ) ) ;
#12602 = CARTESIAN_POINT ( 'NONE',  ( -145.6429501568359797, -168.8438272943107563, 57.67623309621198047 ) ) ;
#12603 = CARTESIAN_POINT ( 'NONE',  ( 32.31036143884366396, 152.4250368413922274, -10.51794503956956817 ) ) ;
#12604 = CARTESIAN_POINT ( 'NONE',  ( -160.8964159109769696, -191.3084106276440650, 46.59394152635518793 ) ) ;
#12605 = ORIENTED_EDGE ( 'NONE', *, *, #10273, .T. ) ;
#12606 = EDGE_CURVE ( 'NONE', #6960, #13046, #19840, .T. ) ;
#12607 = LINE ( 'NONE', #10744, #276 ) ;
#12608 = DIRECTION ( 'NONE',  ( 0.3450121214752278065, -0.9385982292947087080, -0.000000000000000000 ) ) ;
#12609 = CARTESIAN_POINT ( 'NONE',  ( 38.58424406990786082, 138.3797705074273381, 34.21067981925357060 ) ) ;
#12610 = ORIENTED_EDGE ( 'NONE', *, *, #9562, .F. ) ;
#12611 = LINE ( 'NONE', #19333, #7296 ) ;
#12612 =( BOUNDED_CURVE ( )  B_SPLINE_CURVE ( 2, ( #11116, #11218, #17830, #19282, #15961, #19601, #2741, #12881, #17934, #9585, #873, #21373, #19713 ),
 .UNSPECIFIED., .F., .F. ) 
 B_SPLINE_CURVE_WITH_KNOTS ( ( 3, 2, 2, 2, 2, 2, 3 ),
 ( 0.7132352941176470784, 0.7147058823529411908, 0.7176470588235294157, 0.7205882352941176405, 0.7235294117647058654, 0.7264705882352940902, 0.7279411764705882026 ),
 .UNSPECIFIED. ) 
 CURVE ( )  GEOMETRIC_REPRESENTATION_ITEM ( )  RATIONAL_B_SPLINE_CURVE ( ( 0.9755282581475768211, 0.9755282581475768211, 1.000000000000000000, 0.9510565162951535312, 1.000000000000000000, 0.9510565162951535312, 1.000000000000000000, 0.9510565162951535312, 1.000000000000000000, 0.9510565162951535312, 1.000000000000000000, 0.9755282581475768211, 0.9755282581475768211 ) ) 
 REPRESENTATION_ITEM ( '' )  );
#12613 = ORIENTED_EDGE ( 'NONE', *, *, #12992, .F. ) ;
#12614 = CARTESIAN_POINT ( 'NONE',  ( 46.59305225739526435, 124.5797705074273267, 36.81289934271958941 ) ) ;
#12615 = DIRECTION ( 'NONE',  ( 0.5000000000000002220, 0.000000000000000000, -0.8660254037844384856 ) ) ;
#12616 = PLANE ( 'NONE',  #6634 ) ;
#12617 = CARTESIAN_POINT ( 'NONE',  ( 43.01140435219951286, 130.4604996726487229, 39.21067981925356349 ) ) ;
#12618 = CARTESIAN_POINT ( 'NONE',  ( 38.96631938032478359, 159.4104996726487400, 31.27175355779120025 ) ) ;
#12619 = CARTESIAN_POINT ( 'NONE',  ( -157.6495955161842062, -188.0391397928654555, 58.16351966513671812 ) ) ;
#12620 = CARTESIAN_POINT ( 'NONE',  ( 44.55648932407425633, 132.6844580088725820, 38.96596240072933170 ) ) ;
#12621 = CARTESIAN_POINT ( 'NONE',  ( 48.01140435219951996, 125.2104996726487514, 34.21067981925357060 ) ) ;
#12622 = CARTESIAN_POINT ( 'NONE',  ( -154.5594255724347761, -162.9630981290893317, 59.16757674456785310 ) ) ;
#12623 = PRODUCT_CONTEXT ( 'NONE', #12376, 'mechanical' ) ;
#12624 = CARTESIAN_POINT ( 'NONE',  ( 46.10157429594899270, 109.7344580088725650, 29.95742577749336988 ) ) ;
#12625 = CARTESIAN_POINT ( 'NONE',  ( 44.55648932407425633, 135.6844580088725820, 38.96596240072933170 ) ) ;
#12626 = CARTESIAN_POINT ( 'NONE',  ( 44.37947211624943833, 113.4797705074273324, 30.00020018409699318 ) ) ;
#12627 = CARTESIAN_POINT ( 'NONE',  ( 65.02109649036992778, 137.6666368931563227, 10.91413209638136728 ) ) ;
#12628 = CARTESIAN_POINT ( 'NONE',  ( 43.01140435219951996, 10.71049967264875491, 29.21067981925357060 ) ) ;
#12629 = CARTESIAN_POINT ( 'NONE',  ( 40.27526882409969744, 95.66518717409398675, 30.44471234641812174 ) ) ;
#12630 = CARTESIAN_POINT ( 'NONE',  ( 38.01140435219952707, 90.56049967264874567, 32.58608133808903773 ) ) ;
#12631 = VERTEX_POINT ( 'NONE', #11566 ) ;
#12632 = ADVANCED_FACE ( 'NONE', ( #15317 ), #21720, .F. ) ;
#12633 = CARTESIAN_POINT ( 'NONE',  ( 46.10157429594899270, 75.83445800887257349, 38.46393386101375711 ) ) ;
#12634 = CARTESIAN_POINT ( 'NONE',  ( 26.90790578767411390, 150.1165885900122987, 3.291480155758420345 ) ) ;
#12635 = CARTESIAN_POINT ( 'NONE',  ( 34.40470276422951912, 146.6778736915268553, -16.43444041970612446 ) ) ;
#12636 = CARTESIAN_POINT ( 'NONE',  ( 0.000000000000000000, 0.000000000000000000, -29.99999999999997868 ) ) ;
#12637 = CARTESIAN_POINT ( 'NONE',  ( 43.01140435219951286, 76.12977050742732388, 38.86567161673127657 ) ) ;
#12638 = ORIENTED_EDGE ( 'NONE', *, *, #16551, .T. ) ;
#12639 = EDGE_LOOP ( 'NONE', ( #8540, #9969, #9128, #12333 ) ) ;
#12640 = CARTESIAN_POINT ( 'NONE',  ( 40.27526882409969033, 158.9297705074272642, 30.44471234641811819 ) ) ;
#12641 = AXIS2_PLACEMENT_3D ( 'NONE', #11553, #2957, #19945 ) ;
#12642 = CARTESIAN_POINT ( 'NONE',  ( 43.01140435219951286, 120.5344580088725763, 39.21067981925356349 ) ) ;
#12643 = CARTESIAN_POINT ( 'NONE',  ( 48.01140435219951996, 119.3604996726487570, 32.58608133808903773 ) ) ;
#12645 = CARTESIAN_POINT ( 'NONE',  ( 14.34121205894687456, 138.4663445754194697, 3.724531598165178092 ) ) ;
#12644 = CARTESIAN_POINT ( 'NONE',  ( 45.74753988029933538, 73.16518717409400097, 37.97664729208901946 ) ) ;
#12646 = CARTESIAN_POINT ( 'NONE',  ( -154.3824083646099439, -170.4938272943107336, 40.69124936498395328 ) ) ;
#12647 = CARTESIAN_POINT ( 'NONE',  ( 48.01140435219951996, 113.0604996726487315, 35.83527830041809636 ) ) ;
#12648 = CARTESIAN_POINT ( 'NONE',  ( -148.3790856849358306, -188.4630981290893317, 40.14644641866477315 ) ) ;
#12649 = FACE_OUTER_BOUND ( 'NONE', #10209, .T. ) ;
#12650 = CARTESIAN_POINT ( 'NONE',  ( 48.01140435219951996, 157.4344580088725536, 32.58608133808903773 ) ) ;
#12651 = CARTESIAN_POINT ( 'NONE',  ( 39.42975644700377558, 144.0797705074273267, 31.60846029578754468 ) ) ;
#12652 = CARTESIAN_POINT ( 'NONE',  ( 20.33033954036769941, 94.15838586645493535, 7.144317217164116052 ) ) ;
#12653 = CARTESIAN_POINT ( 'NONE',  ( 45.74753988029934249, 124.1651871740940152, 37.97664729208901235 ) ) ;
#12654 = EDGE_CURVE ( 'NONE', #14419, #6804, #19367, .T. ) ;
#12655 = DIRECTION ( 'NONE',  ( 1.000000000000000000, 0.000000000000000000, 0.000000000000000000 ) ) ;
#12656 = CARTESIAN_POINT ( 'NONE',  ( -160.8964159109769696, -158.1584106276440593, 49.65701158161630957 ) ) ;
#12657 = AXIS2_PLACEMENT_3D ( 'NONE', #2403, #7050, #17169 ) ;
#12658 = CARTESIAN_POINT ( 'NONE',  ( -154.5594255724347761, -165.0891397928654669, 40.14644641866476604 ) ) ;
#12659 = CARTESIAN_POINT ( 'NONE',  ( -153.0531000319306827, -156.1622583705452030, 39.65701158161629536 ) ) ;
#12660 = CARTESIAN_POINT ( 'NONE',  ( 67.88957565821384321, 106.4565162521658976, 12.22353771717463466 ) ) ;
#12661 = CARTESIAN_POINT ( 'NONE',  ( 0.000000000000000000, 160.7104996726487514, -25.00000000000000000 ) ) ;
#12662 = CARTESIAN_POINT ( 'NONE',  ( 43.01140435219951286, 105.8651871740939754, 38.86567161673127657 ) ) ;
#12663 = ORIENTED_EDGE ( 'NONE', *, *, #7587, .T. ) ;
#12664 = FACE_OUTER_BOUND ( 'NONE', #19201, .T. ) ;
#12665 = ORIENTED_EDGE ( 'NONE', *, *, #21546, .F. ) ;
#12666 = CARTESIAN_POINT ( 'NONE',  ( 41.46631938032478359, 89.18445800887258201, 29.45539723777780239 ) ) ;
#12667 = CARTESIAN_POINT ( 'NONE',  ( 54.85617982533818804, 239.2521282348021714, -3.999999999999980904 ) ) ;
#12668 = PRODUCT_DEFINITION_FORMATION_WITH_SPECIFIED_SOURCE ( 'ANY', '', #6419, .NOT_KNOWN. ) ;
#12669 = CARTESIAN_POINT ( 'NONE',  ( 39.92123440845004723, 153.2604996726487343, 29.95742577749337343 ) ) ;
#12671 = CARTESIAN_POINT ( 'NONE',  ( 16.34080065753823163, 110.9948608346959276, -11.19624206051981474 ) ) ;
#12670 = CARTESIAN_POINT ( 'NONE',  ( 40.27526882409969033, 107.6651871740940152, 30.44471234641811819 ) ) ;
#12672 = CARTESIAN_POINT ( 'NONE',  ( 41.46631938032478359, 66.11049967264874283, 29.45539723777780239 ) ) ;
#12674 = CARTESIAN_POINT ( 'NONE',  ( 48.01140435219951996, 61.43445800887257491, 32.58608133808903773 ) ) ;
#12673 = CYLINDRICAL_SURFACE ( 'NONE', #21022, 2.999999999999997780 ) ;
#12675 = DIRECTION ( 'NONE',  ( 0.000000000000000000, 0.000000000000000000, 1.000000000000000000 ) ) ;
#12676 = DIRECTION ( 'NONE',  ( 0.000000000000000000, 0.000000000000000000, 1.000000000000000000 ) ) ;
#12677 = CARTESIAN_POINT ( 'NONE',  ( 33.56091001181424360, 87.00402361476987778, -6.351118090676544981 ) ) ;
#12678 = FACE_OUTER_BOUND ( 'NONE', #3408, .T. ) ;
#12679 = CARTESIAN_POINT ( 'NONE',  ( -154.3824083646099439, -167.4938272943107336, 40.69124936498395328 ) ) ;
#12680 = CARTESIAN_POINT ( 'NONE',  ( -143.8425227516148084, -195.3584106276440480, 44.11586579668791330 ) ) ;
#12681 = VERTEX_POINT ( 'NONE', #16741 ) ;
#12682 = CARTESIAN_POINT ( 'NONE',  ( 37.02312590732701381, 153.6946607573816834, 9.644493012478044136 ) ) ;
#12683 = VERTEX_POINT ( 'NONE', #11450 ) ;
#12684 = CARTESIAN_POINT ( 'NONE',  ( 46.59305225739526435, 136.9151871740940010, 31.60846029578754468 ) ) ;
#12685 = PRESENTATION_LAYER_ASSIGNMENT (  '', '', ( #18325 ) ) ;
#12686 = EDGE_CURVE ( 'NONE', #6094, #310, #16632, .T. ) ;
#12687 = CARTESIAN_POINT ( 'NONE',  ( 47.43856463449118621, 97.87977050742732388, 34.21067981925357060 ) ) ;
#12688 = ORIENTED_EDGE ( 'NONE', *, *, #10518, .T. ) ;
#12689 = ORIENTED_EDGE ( 'NONE', *, *, #19108, .F. ) ;
#12690 = CARTESIAN_POINT ( 'NONE',  ( 15.80414578680225723, 112.4924633436790344, 15.87081086175909306 ) ) ;
#12691 = VERTEX_POINT ( 'NONE', #3292 ) ;
#12692 = CARTESIAN_POINT ( 'NONE',  ( 44.55648932407425633, 111.6844580088725820, 38.96596240072933170 ) ) ;
#12693 = PRODUCT_RELATED_PRODUCT_CATEGORY ( 'part', '', ( #15187 ) ) ;
#12694 = CARTESIAN_POINT ( 'NONE',  ( 43.80332655382220253, 89.88361825032846752, 29.21067981925356705 ) ) ;
#12695 = CARTESIAN_POINT ( 'NONE',  ( 41.64333658814960870, 74.77977050742731535, 30.00020018409699318 ) ) ;
#12696 = CARTESIAN_POINT ( 'NONE',  ( 47.43856463449117200, 139.4651871740940123, 35.64915139335016647 ) ) ;
#12697 = CARTESIAN_POINT ( 'NONE',  ( 39.92123440845004723, 90.26049967264873430, 29.95742577749337343 ) ) ;
#12698 = CARTESIAN_POINT ( 'NONE',  ( 63.41425016244589585, 92.41789933959738335, 6.624947895572852019 ) ) ;
#12699 = EDGE_CURVE ( 'NONE', #13046, #16234, #10020, .T. ) ;
#12700 = CARTESIAN_POINT ( 'NONE',  ( 41.39091152515459271, 94.95783073190082746, 38.95199156105032046 ) ) ;
#12701 = CARTESIAN_POINT ( 'NONE',  ( -151.4692556286852891, -165.2391397928654442, 39.14238933923362396 ) ) ;
#12702 = CARTESIAN_POINT ( 'NONE',  ( -151.4692556286852607, -158.3130981290892692, 39.65701158161629536 ) ) ;
#12703 = DIRECTION ( 'NONE',  ( 0.000000000000000000, 1.000000000000000000, 0.000000000000000000 ) ) ;
#12704 = CARTESIAN_POINT ( 'NONE',  ( -151.4692556286853176, -162.8130981290893260, 59.65701158161632378 ) ) ;
#12705 = ORIENTED_EDGE ( 'NONE', *, *, #11834, .T. ) ;
#12706 = CARTESIAN_POINT ( 'NONE',  ( 47.43856463449117200, 73.72977050742731819, 35.64915139335016647 ) ) ;
#12707 = CARTESIAN_POINT ( 'NONE',  ( -154.3824083646099439, -164.4938272943107336, 40.69124936498395328 ) ) ;
#12708 = EDGE_CURVE ( 'NONE', #19941, #10182, #5190, .T. ) ;
#12709 = CARTESIAN_POINT ( 'NONE',  ( 51.60797029699607918, 86.77139250312444574, -6.946567135388369785 ) ) ;
#12710 = CARTESIAN_POINT ( 'NONE',  ( -159.0959885057557983, -193.8584106276440480, 55.19815736654470584 ) ) ;
#12711 = ORIENTED_EDGE ( 'NONE', *, *, #13822, .T. ) ;
#12712 = DIRECTION ( 'NONE',  ( 0.000000000000000000, 0.000000000000000000, -1.000000000000000000 ) ) ;
#12713 = CARTESIAN_POINT ( 'NONE',  ( -151.4692556286852891, -196.9891397928655010, 49.65701158161630957 ) ) ;
#12714 = CARTESIAN_POINT ( 'NONE',  ( 47.43856463449118621, 127.8797705074273239, 34.21067981925357060 ) ) ;
#12715 = EDGE_CURVE ( 'NONE', #17523, #3649, #13295, .T. ) ;
#12716 = ORIENTED_EDGE ( 'NONE', *, *, #3684, .F. ) ;
#12717 = CARTESIAN_POINT ( 'NONE',  ( 44.55648932407425633, 129.6844580088725820, 38.96596240072933170 ) ) ;
#12718 = ORIENTED_EDGE ( 'NONE', *, *, #10314, .F. ) ;
#12719 = CARTESIAN_POINT ( 'NONE',  ( 45.74753988029933538, 122.3297705074273267, 30.44471234641811819 ) ) ;
#12720 = CARTESIAN_POINT ( 'NONE',  ( 43.80332655382221674, 109.5373810949689926, 39.21067981925355639 ) ) ;
#12721 = CARTESIAN_POINT ( 'NONE',  ( 43.01140435219951286, 60.53445800887259054, 39.46799094044489209 ) ) ;
#12722 = VECTOR ( 'NONE', #16781, 1000.000000000000000 ) ;
#12723 = CARTESIAN_POINT ( 'NONE',  ( 38.01140435219952707, 110.6344580088725849, 32.58608133808903773 ) ) ;
#12724 = CARTESIAN_POINT ( 'NONE',  ( 43.01140435219951286, 84.53445800887256212, 39.21067981925356349 ) ) ;
#12725 = DIRECTION ( 'NONE',  ( 0.000000000000000000, 0.000000000000000000, 1.000000000000000000 ) ) ;
#12726 = CARTESIAN_POINT ( 'NONE',  ( -145.2889157411863721, -192.5391397928654840, 41.15050349809590102 ) ) ;
#12727 = CARTESIAN_POINT ( 'NONE',  ( 38.01140435219952707, 66.86049967264872862, 35.83527830041809636 ) ) ;
#12728 = DIRECTION ( 'NONE',  ( 0.3428981916074316239, -0.9393725726208708160, -0.000000000000000000 ) ) ;
#12729 = CARTESIAN_POINT ( 'NONE',  ( -161.4692556286853176, -163.5630981290893260, 49.65701158161630957 ) ) ;
#12730 = AXIS2_PLACEMENT_3D ( 'NONE', #1510, #18259, #17916 ) ;
#12731 = ADVANCED_FACE ( 'NONE', ( #19942, #15192, #19824, #16835 ), #20269, .T. ) ;
#12732 = CARTESIAN_POINT ( 'NONE',  ( 38.96631938032478359, 131.4844580088725934, 31.27175355779120025 ) ) ;
#12733 = CARTESIAN_POINT ( 'NONE',  ( 41.64333658814960870, 102.9797705074273182, 38.42115945441014446 ) ) ;
#12734 = CARTESIAN_POINT ( 'NONE',  ( 62.80402591640378773, 99.70611228127967252, 5.556743651330835476 ) ) ;
#12735 = CARTESIAN_POINT ( 'NONE',  ( -154.3824083646099439, -193.2938272943107449, 58.62277379824867296 ) ) ;
#12736 = CARTESIAN_POINT ( 'NONE',  ( 38.58424406990785371, 95.96518717409396970, 32.77220824515697473 ) ) ;
#12737 = CARTESIAN_POINT ( 'NONE',  ( -151.4692556286852607, -161.3130981290892976, 39.65701158161629536 ) ) ;
#12738 = ORIENTED_EDGE ( 'NONE', *, *, #7925, .T. ) ;
#12739 = CARTESIAN_POINT ( 'NONE',  ( 46.10157429594899270, 127.7604996726487485, 38.46393386101375711 ) ) ;
#12740 = CARTESIAN_POINT ( 'NONE',  ( 76.92284642892752800, 124.5854180935290714, 5.434424407683230207 ) ) ;
#12741 =( BOUNDED_CURVE ( )  B_SPLINE_CURVE ( 2, ( #17840, #17626, #17948, #9269, #667, #15970, #11125, #20840, #7404, #7728, #12456, #12780, #881 ),
 .UNSPECIFIED., .F., .F. ) 
 B_SPLINE_CURVE_WITH_KNOTS ( ( 3, 2, 2, 2, 2, 2, 3 ),
 ( 0.8750000000000000000, 0.8785714285714285587, 0.8857142857142856762, 0.8928571428571429047, 0.9000000000000000222, 0.9071428571428571397, 0.9107142857142856984 ),
 .UNSPECIFIED. ) 
 CURVE ( )  GEOMETRIC_REPRESENTATION_ITEM ( )  RATIONAL_B_SPLINE_CURVE ( ( 0.9755282581475768211, 0.9755282581475768211, 1.000000000000000000, 0.9510565162951535312, 1.000000000000000000, 0.9510565162951535312, 1.000000000000000000, 0.9510565162951535312, 1.000000000000000000, 0.9510565162951535312, 1.000000000000000000, 0.9755282581475768211, 0.9755282581475768211 ) ) 
 REPRESENTATION_ITEM ( '' )  );
#12742 = CARTESIAN_POINT ( 'NONE',  ( 31.57890723221301599, 145.5991046824261446, -16.55366158474257432 ) ) ;
#12743 = CARTESIAN_POINT ( 'NONE',  ( 76.20123706073158587, 111.5182621349952257, -8.137091297256032973 ) ) ;
#12744 = AXIS2_PLACEMENT_3D ( 'NONE', #13925, #2143, #10529 ) ;
#12745 = CARTESIAN_POINT ( 'NONE',  ( 38.58424406990785371, 81.22977050742731819, 32.77220824515697473 ) ) ;
#12746 = ORIENTED_EDGE ( 'NONE', *, *, #5154, .T. ) ;
#12747 = ORIENTED_EDGE ( 'NONE', *, *, #2011, .F. ) ;
#12748 = CARTESIAN_POINT ( 'NONE',  ( 45.74753988029933538, 152.3297705074272699, 30.44471234641811819 ) ) ;
#12749 = AXIS2_PLACEMENT_3D ( 'NONE', #13736, #20474, #3718 ) ;
#12750 = EDGE_CURVE ( 'NONE', #15251, #872, #16451, .T. ) ;
#12751 = CARTESIAN_POINT ( 'NONE',  ( 38.96631938032478359, 118.0104996726487485, 37.14960608071593384 ) ) ;
#12753 = CARTESIAN_POINT ( 'NONE',  ( 70.84804472268019992, 100.1183116193850964, 0.2719452077637916076 ) ) ;
#12752 = CARTESIAN_POINT ( 'NONE',  ( 39.42975644700377558, 75.41518717409400097, 36.81289934271958941 ) ) ;
#12754 = CARTESIAN_POINT ( 'NONE',  ( -157.2955611005345986, -169.4438272943106938, 57.67623309621197336 ) ) ;
#12755 = LINE ( 'NONE', #7483, #2641 ) ;
#12756 = CARTESIAN_POINT ( 'NONE',  ( -145.2889157411863721, -186.5130981290893430, 58.16351966513671812 ) ) ;
#12757 = DIRECTION ( 'NONE',  ( 0.000000000000000000, 1.000000000000000000, 0.000000000000000000 ) ) ;
#12758 = CARTESIAN_POINT ( 'NONE',  ( 43.01140435219951996, 149.0344580088725763, 29.21067981925357060 ) ) ;
#12759 = CARTESIAN_POINT ( 'NONE',  ( 47.43856463449117200, 133.7297705074273324, 35.64915139335016647 ) ) ;
#12760 = CARTESIAN_POINT ( 'NONE',  ( 17.52475135776945336, 142.8823211630961794, 1.906181796079885027 ) ) ;
#12761 = CARTESIAN_POINT ( 'NONE',  ( 41.64333658814960870, 126.7151871740939981, 38.42115945441014446 ) ) ;
#12762 = CARTESIAN_POINT ( 'NONE',  ( 48.01140435219951996, 137.0604996726487457, 35.83527830041809636 ) ) ;
#12763 = CARTESIAN_POINT ( 'NONE',  ( -142.0420953463935803, -156.8084106276440366, 52.72008163687743831 ) ) ;
#12764 = CARTESIAN_POINT ( 'NONE',  ( 38.58424406990784661, 60.22977050742731109, 32.77220824515698183 ) ) ;
#12765 = CARTESIAN_POINT ( 'NONE',  ( 43.01140435219951286, 134.9604996726487514, 29.21067981925356705 ) ) ;
#12766 = CARTESIAN_POINT ( 'NONE',  ( 25.76509531087978289, 97.49384569152056201, 21.15186415193267067 ) ) ;
#12767 = FACE_OUTER_BOUND ( 'NONE', #12798, .T. ) ;
#12768 = CARTESIAN_POINT ( 'NONE',  ( 38.58424406990786082, 105.1151871740940038, 34.21067981925357060 ) ) ;
#12769 = VERTEX_POINT ( 'NONE', #20167 ) ;
#12770 = CARTESIAN_POINT ( 'NONE',  ( 26.17254549292281496, -61.68114226949890622, -16.21320343559643717 ) ) ;
#12771 = ORIENTED_EDGE ( 'NONE', *, *, #3662, .T. ) ;
#12772 = CARTESIAN_POINT ( 'NONE',  ( 46.10157429594899270, 90.83445800887255928, 38.46393386101376421 ) ) ;
#12773 = PLANE ( 'NONE',  #9835 ) ;
#12774 = EDGE_CURVE ( 'NONE', #13802, #846, #5056, .T. ) ;
#12775 = CARTESIAN_POINT ( 'NONE',  ( 44.55648932407425633, 149.8104996726487457, 29.45539723777780239 ) ) ;
#12777 = CARTESIAN_POINT ( 'NONE',  ( 22.37680805599060818, 139.0098026693046336, -10.00581381704545514 ) ) ;
#12776 = CARTESIAN_POINT ( 'NONE',  ( 46.59305225739526435, 106.3151871740939924, 36.81289934271958941 ) ) ;
#12778 = CARTESIAN_POINT ( 'NONE',  ( 47.05648932407426344, 61.91049967264873288, 37.14960608071593384 ) ) ;
#12780 = CARTESIAN_POINT ( 'NONE',  ( -153.0531000319306827, -156.8899795514095672, 59.65701158161631668 ) ) ;
#12779 = DIRECTION ( 'NONE',  ( 1.000000000000000000, 0.000000000000000000, 0.000000000000000000 ) ) ;
#12781 = CARTESIAN_POINT ( 'NONE',  ( 43.80332655382220253, 118.9575765865522925, 29.21067981925356705 ) ) ;
#12782 = CARTESIAN_POINT ( 'NONE',  ( 151.4773229304660731, 84.89323405393692212, 14.00000000000001776 ) ) ;
#12783 = LINE ( 'NONE', #10921, #12245 ) ;
#12784 = CARTESIAN_POINT ( 'NONE',  ( 41.64333658814960870, 69.71518717409399812, 38.42115945441014446 ) ) ;
#12785 = CARTESIAN_POINT ( 'NONE',  ( 57.94507594753278568, 150.7106492751291569, -2.660852849641732298 ) ) ;
#12786 = EDGE_CURVE ( 'NONE', #10404, #1447, #4300, .T. ) ;
#12787 = CARTESIAN_POINT ( 'NONE',  ( 38.58424406990786082, 153.1151871740939896, 34.21067981925357060 ) ) ;
#12788 = CARTESIAN_POINT ( 'NONE',  ( -151.4692556286852607, -155.3130981290892976, 39.65701158161629536 ) ) ;
#12789 = CARTESIAN_POINT ( 'NONE',  ( -154.3824083646099439, -175.2938272943107165, 58.62277379824867296 ) ) ;
#12790 = CARTESIAN_POINT ( 'NONE',  ( -148.5561028927606344, -181.2584106276440536, 58.62277379824867296 ) ) ;
#12791 = ORIENTED_EDGE ( 'NONE', *, *, #11107, .F. ) ;
#12792 = CARTESIAN_POINT ( 'NONE',  ( -157.2955611005346270, -167.6084106276440480, 41.63779006702063867 ) ) ;
#12793 = CARTESIAN_POINT ( 'NONE',  ( 53.94306145151312393, 87.38125778962682944, 12.97772928308168616 ) ) ;
#12794 = VERTEX_POINT ( 'NONE', #8367 ) ;
#12795 = CARTESIAN_POINT ( 'NONE',  ( 41.64333658814960870, 134.5151871740939953, 30.00020018409699318 ) ) ;
#12796 = CARTESIAN_POINT ( 'NONE',  ( 46.59305225739526435, 154.9151871740940010, 31.60846029578754468 ) ) ;
#12797 = CARTESIAN_POINT ( 'NONE',  ( 47.43856463449117911, 92.02977050742730114, 32.77220824515697473 ) ) ;
#12798 = EDGE_LOOP ( 'NONE', ( #16014, #7854, #14446, #16779 ) ) ;
#12799 = ORIENTED_EDGE ( 'NONE', *, *, #4984, .T. ) ;
#12800 = APPLICATION_CONTEXT ( 'automotive_design' ) ;
#12801 = CARTESIAN_POINT ( 'NONE',  ( -151.4692556286852607, -192.2391397928655010, 39.65701158161629536 ) ) ;
#12802 = ORIENTED_EDGE ( 'NONE', *, *, #19592, .T. ) ;
#12803 = CARTESIAN_POINT ( 'NONE',  ( 54.85617982533816672, 239.2521282348021714, -19.99999999999996092 ) ) ;
#12804 = CARTESIAN_POINT ( 'NONE',  ( 45.74753988029933538, 79.42977050742732104, 37.97664729208901946 ) ) ;
#12805 = CARTESIAN_POINT ( 'NONE',  ( 47.43856463449117200, 130.7651871740939953, 32.77220824515698183 ) ) ;
#12806 = CARTESIAN_POINT ( 'NONE',  ( 38.01140435219951996, 87.86049967264871441, 35.83527830041810347 ) ) ;
#12807 = CARTESIAN_POINT ( 'NONE',  ( 72.33162239183086228, 137.5781058455011703, 11.98183203572534872 ) ) ;
#12808 = CARTESIAN_POINT ( 'NONE',  ( 39.95954646485986927, 95.09254297023964853, 30.23659822568392386 ) ) ;
#12809 = CARTESIAN_POINT ( 'NONE',  ( -145.2889157411863721, -159.5391397928654840, 41.15050349809590102 ) ) ;
#12810 = ADVANCED_FACE ( 'NONE', ( #4714 ), #10239, .T. ) ;
#12811 = LINE ( 'NONE', #11155, #18914 ) ;
#12812 = CARTESIAN_POINT ( 'NONE',  ( 43.80332655382221674, 141.6113394311928744, 39.21067981925356349 ) ) ;
#12813 = VERTEX_POINT ( 'NONE', #16500 ) ;
#12814 = CARTESIAN_POINT ( 'NONE',  ( 45.74753988029933538, 73.42977050742732104, 37.97664729208901946 ) ) ;
#12815 = CARTESIAN_POINT ( 'NONE',  ( -148.5561028927606344, -156.9938272943107052, 58.62277379824867296 ) ) ;
#12816 = CARTESIAN_POINT ( 'NONE',  ( 61.61057083318216598, 91.16763906547615193, -7.303593892219363504 ) ) ;
#12817 = CARTESIAN_POINT ( 'NONE',  ( -157.2955611005346270, -184.7084106276440423, 57.67623309621198047 ) ) ;
#12818 = EDGE_LOOP ( 'NONE', ( #9631, #7444 ) ) ;
#12819 = DIRECTION ( 'NONE',  ( -0.000000000000000000, 0.000000000000000000, -1.000000000000000000 ) ) ;
#12820 = CARTESIAN_POINT ( 'NONE',  ( 43.01140435219951286, 104.0344580088725763, 29.21067981925356705 ) ) ;
#12821 = VECTOR ( 'NONE', #1430, 1000.000000000000000 ) ;
#12822 = CARTESIAN_POINT ( 'NONE',  ( 40.27526882409969744, 122.9297705074273068, 30.44471234641812174 ) ) ;
#12823 = ORIENTED_EDGE ( 'NONE', *, *, #14589, .T. ) ;
#12824 = AXIS2_PLACEMENT_3D ( 'NONE', #2294, #2089, #17281 ) ;
#12825 = ORIENTED_EDGE ( 'NONE', *, *, #12414, .F. ) ;
#12826 = CARTESIAN_POINT ( 'NONE',  ( 38.58424406990786082, 126.3797705074273239, 34.21067981925357060 ) ) ;
#12827 = CARTESIAN_POINT ( 'NONE',  ( -136.4581486297550441, -126.9891397928655010, 49.65701158161631668 ) ) ;
#12828 = CARTESIAN_POINT ( 'NONE',  ( 43.01140435219951286, 89.62977050742729546, 29.55568802177586463 ) ) ;
#12829 = CARTESIAN_POINT ( 'NONE',  ( 38.96631938032478359, 63.08445800887258059, 37.14960608071593384 ) ) ;
#12830 = EDGE_CURVE ( 'NONE', #15106, #17048, #4828, .T. ) ;
#12831 = CARTESIAN_POINT ( 'NONE',  ( 43.01140435219951996, 10.71049967264875491, 39.21067981925356349 ) ) ;
#12832 = DIRECTION ( 'NONE',  ( 1.000000000000000000, 0.000000000000000000, 0.000000000000000000 ) ) ;
#12833 = CARTESIAN_POINT ( 'NONE',  ( 43.01140435219957681, 97.46049967264875136, 39.21067981925356349 ) ) ;
#12834 = CARTESIAN_POINT ( 'NONE',  ( -145.2889157411863721, -189.5391397928654271, 41.15050349809590102 ) ) ;
#12835 = CARTESIAN_POINT ( 'NONE',  ( 38.96631938032478359, 67.01049967264874851, 37.14960608071593384 ) ) ;
#12836 = CARTESIAN_POINT ( 'NONE',  ( 46.10157429594899270, 93.83445800887257349, 38.46393386101375711 ) ) ;
#12837 = CARTESIAN_POINT ( 'NONE',  ( -142.0420953463935803, -186.5438272943107449, 52.72008163687743831 ) ) ;
#12838 = APPLICATION_PROTOCOL_DEFINITION ( 'draft international standard', 'automotive_design', 1998, #1833 ) ;
#12839 = CARTESIAN_POINT ( 'NONE',  ( 43.01140435219951286, 122.0344580088725621, 28.95336869806222779 ) ) ;
#12840 = CARTESIAN_POINT ( 'NONE',  ( 38.58424406990784661, 105.5297705074273011, 35.64915139335016647 ) ) ;
#12841 = CARTESIAN_POINT ( 'NONE',  ( 24.55476856798156859, 141.3345980244743885, 9.128255474432329208 ) ) ;
#12842 = CARTESIAN_POINT ( 'NONE',  ( -145.6429501568359797, -182.9438272943106938, 41.63779006702063867 ) ) ;
#12843 = CARTESIAN_POINT ( 'NONE',  ( 43.01140435219951286, 96.86518717409398960, 38.86567161673127657 ) ) ;
#12844 = CARTESIAN_POINT ( 'NONE',  ( -148.3790856849358306, -161.4630981290893317, 40.14644641866477315 ) ) ;
#12845 = ORIENTED_EDGE ( 'NONE', *, *, #14009, .F. ) ;
#12846 = CARTESIAN_POINT ( 'NONE',  ( 163.4517194221884040, 198.8869265230379995, 272.0939500981630204 ) ) ;
#12847 = CARTESIAN_POINT ( 'NONE',  ( 69.27296957579615366, 97.94681810169329594, -0.6368323762655749842 ) ) ;
#12848 = CARTESIAN_POINT ( 'NONE',  ( 60.50179475597519740, 141.9260456451392827, -8.339099203377070779 ) ) ;
#12849 = CARTESIAN_POINT ( 'NONE',  ( 39.42975644700377558, 66.07977050742731251, 31.60846029578754468 ) ) ;
#12850 = VERTEX_POINT ( 'NONE', #21596 ) ;
#12851 = VERTEX_POINT ( 'NONE', #3407 ) ;
#12852 = CARTESIAN_POINT ( 'NONE',  ( 43.01140435219951286, 152.6297705074272812, 29.55568802177586463 ) ) ;
#12854 = ADVANCED_FACE ( 'NONE', ( #11550 ), #18279, .F. ) ;
#12853 = CARTESIAN_POINT ( 'NONE',  ( -159.5594255724347761, -193.8630981290893089, 43.77915905869157598 ) ) ;
#12855 = AXIS2_PLACEMENT_3D ( 'NONE', #844, #15933, #12196 ) ;
#12856 = CARTESIAN_POINT ( 'NONE',  ( 39.92123440845004723, 118.1604996726487542, 38.46393386101376421 ) ) ;
#12858 = CARTESIAN_POINT ( 'NONE',  ( 76.37589548207274959, 127.2077353526990748, 6.343625931721379452 ) ) ;
#12857 = CARTESIAN_POINT ( 'NONE',  ( 44.37947211624943833, 71.21518717409399812, 30.00020018409699318 ) ) ;
#12859 = CARTESIAN_POINT ( 'NONE',  ( 38.01140435219952707, 65.78445800887257633, 34.21067981925357060 ) ) ;
#12860 = CARTESIAN_POINT ( 'NONE',  ( -160.8964159109769696, -173.0438272943107165, 46.59394152635518083 ) ) ;
#12861 = CARTESIAN_POINT ( 'NONE',  ( 11.08170843061617816, 132.1625483722078513, 16.49545033792581350 ) ) ;
#12862 = CARTESIAN_POINT ( 'NONE',  ( -141.4692556286852891, -179.9130981290893487, 46.40781461928724383 ) ) ;
#12863 =( NAMED_UNIT ( * ) SI_UNIT ( $, .STERADIAN. ) SOLID_ANGLE_UNIT ( ) );
#12864 = FACE_BOUND ( 'NONE', #16533, .T. ) ;
#12865 = FACE_OUTER_BOUND ( 'NONE', #16208, .T. ) ;
#12866 = CARTESIAN_POINT ( 'NONE',  ( 40.27526882409969033, 134.9297705074272926, 30.44471234641811819 ) ) ;
#12867 =( BOUNDED_CURVE ( )  B_SPLINE_CURVE ( 2, ( #10555, #3829, #5903, #20798, #4043, #945, #10978, #2593, #17691, #737, #6010, #626, #5690 ),
 .UNSPECIFIED., .F., .F. ) 
 B_SPLINE_CURVE_WITH_KNOTS ( ( 3, 2, 2, 2, 2, 2, 3 ),
 ( 0.6985294117647058432, 0.6999999999999999556, 0.7029411764705881804, 0.7058823529411765163, 0.7088235294117647411, 0.7117647058823529660, 0.7132352941176470784 ),
 .UNSPECIFIED. ) 
 CURVE ( )  GEOMETRIC_REPRESENTATION_ITEM ( )  RATIONAL_B_SPLINE_CURVE ( ( 0.9755282581475768211, 0.9755282581475768211, 1.000000000000000000, 0.9510565162951535312, 1.000000000000000000, 0.9510565162951535312, 1.000000000000000000, 0.9510565162951535312, 1.000000000000000000, 0.9510565162951535312, 1.000000000000000000, 0.9755282581475768211, 0.9755282581475768211 ) ) 
 REPRESENTATION_ITEM ( '' )  );
#12868 = EDGE_CURVE ( 'NONE', #6293, #12132, #10372, .T. ) ;
#12869 = CARTESIAN_POINT ( 'NONE',  ( 9.529548018246485341, 127.4200721877477491, 8.334841288026581196 ) ) ;
#12870 = CARTESIAN_POINT ( 'NONE',  ( 40.27526882409969744, 129.5651871740940067, 37.97664729208901235 ) ) ;
#12871 = CARTESIAN_POINT ( 'NONE',  ( 38.01140435219952707, 69.56049967264874567, 32.58608133808903773 ) ) ;
#12872 = CARTESIAN_POINT ( 'NONE',  ( -154.3824083646099439, -155.7584106276440536, 40.69124936498395328 ) ) ;
#12873 = CARTESIAN_POINT ( 'NONE',  ( 126.8576204525573274, -136.9891397928655010, -17.64809332337413750 ) ) ;
#12874 = CARTESIAN_POINT ( 'NONE',  ( 43.80332655382220963, 149.8836182503285102, 29.21067981925357060 ) ) ;
#12875 = CARTESIAN_POINT ( 'NONE',  ( 69.45715107853048664, 110.1171555912624740, -7.938611875467805667 ) ) ;
#12876 = AXIS2_PLACEMENT_3D ( 'NONE', #15232, #1678, #8519 ) ;
#12877 = CARTESIAN_POINT ( 'NONE',  ( 43.01140435219951996, 10.71049967264875491, 29.21067981925357060 ) ) ;
#12878 = CARTESIAN_POINT ( 'NONE',  ( 46.59305225739526435, 109.3151871740939924, 36.81289934271958941 ) ) ;
#12879 = EDGE_CURVE ( 'NONE', #4859, #16995, #14152, .T. ) ;
#12880 = ORIENTED_EDGE ( 'NONE', *, *, #10439, .T. ) ;
#12881 = CARTESIAN_POINT ( 'NONE',  ( 48.01140435219951996, 86.06049967264874567, 35.83527830041809636 ) ) ;
#12882 = ORIENTED_EDGE ( 'NONE', *, *, #15389, .T. ) ;
#12883 = CARTESIAN_POINT ( 'NONE',  ( 41.46631938032478359, 80.18445800887258201, 29.45539723777780239 ) ) ;
#12884 = CARTESIAN_POINT ( 'NONE',  ( 43.01140435219951286, 128.9604996726487229, 29.21067981925356705 ) ) ;
#12885 = CARTESIAN_POINT ( 'NONE',  ( 38.01140435219951996, 153.5604996726487173, 32.58608133808903773 ) ) ;
#12887 = CARTESIAN_POINT ( 'NONE',  ( 70.97434162403952485, 116.9407273601718202, 6.779784368693626995 ) ) ;
#12886 = CARTESIAN_POINT ( 'NONE',  ( 46.59305225739526435, 103.9151871740940152, 31.60846029578754468 ) ) ;
#12888 = CARTESIAN_POINT ( 'NONE',  ( 47.05648932407426344, 62.51049967264874141, 31.27175355779120025 ) ) ;
#12890 = CARTESIAN_POINT ( 'NONE',  ( 43.80332655382220963, 147.6113394311928744, 39.21067981925356349 ) ) ;
#12889 = CARTESIAN_POINT ( 'NONE',  ( 47.07948156226018455, 144.5740439970474824, 37.12229684998504808 ) ) ;
#12891 = CARTESIAN_POINT ( 'NONE',  ( 46.10157429594899270, 117.8344580088725593, 38.46393386101375711 ) ) ;
#12892 = AXIS2_PLACEMENT_3D ( 'NONE', #18100, #14361, #7664 ) ;
#12893 = DIRECTION ( 'NONE',  ( 1.000000000000000000, 0.000000000000000000, -0.000000000000000000 ) ) ;
#12894 = CARTESIAN_POINT ( 'NONE',  ( 165.8083469658213005, 192.9029763258799335, -44.99999999999997158 ) ) ;
#12895 = CARTESIAN_POINT ( 'NONE',  ( 47.43856463449118621, 157.8797705074273381, 34.21067981925357060 ) ) ;
#12896 = CARTESIAN_POINT ( 'NONE',  ( 17.73005198514846725, 142.9879744078657779, -4.089424278207452801 ) ) ;
#12897 = CARTESIAN_POINT ( 'NONE',  ( 46.59305225739526435, 151.9151871740940010, 31.60846029578754468 ) ) ;
#12898 = CARTESIAN_POINT ( 'NONE',  ( -151.4692556286852891, -126.9891397928655010, -44.65701158161626694 ) ) ;
#12899 = CARTESIAN_POINT ( 'NONE',  ( -160.8964159109769696, -176.0438272943107165, 46.59394152635518793 ) ) ;
#12900 = CARTESIAN_POINT ( 'NONE',  ( -148.5561028927606344, -189.0584106276440650, 40.69124936498395328 ) ) ;
#12901 = VERTEX_POINT ( 'NONE', #17777 ) ;
#12902 = CARTESIAN_POINT ( 'NONE',  ( 44.37947211624943833, 65.21518717409399812, 30.00020018409699318 ) ) ;
#12903 = CARTESIAN_POINT ( 'NONE',  ( -151.4692556286852891, -166.4084106276440878, 59.56931450028537967 ) ) ;
#12904 = CARTESIAN_POINT ( 'NONE',  ( 76.78854507624612324, 113.8604396784633508, 11.78705480642107517 ) ) ;
#12905 = VECTOR ( 'NONE', #17444, 1000.000000000000000 ) ;
#12906 = CARTESIAN_POINT ( 'NONE',  ( 46.59305225739526435, 130.9151871740940010, 31.60846029578754468 ) ) ;
#12907 = EDGE_CURVE ( 'NONE', #8083, #8428, #13188, .T. ) ;
#12908 = CARTESIAN_POINT ( 'NONE',  ( 17.93535261252752022, 143.0936276526352913, -10.08503035249478685 ) ) ;
#12909 = VECTOR ( 'NONE', #10328, 1000.000000000000114 ) ;
#12910 = VERTEX_POINT ( 'NONE', #5884 ) ;
#12911 = ORIENTED_EDGE ( 'NONE', *, *, #16291, .T. ) ;
#12912 = ORIENTED_EDGE ( 'NONE', *, *, #8265, .T. ) ;
#12913 = CARTESIAN_POINT ( 'NONE',  ( 43.01140435219951286, 116.0344580088725763, 28.95336869806222779 ) ) ;
#12914 = CARTESIAN_POINT ( 'NONE',  ( 156.7804311855217065, 208.8003142469820830, -44.99999999999997158 ) ) ;
#12915 = CARTESIAN_POINT ( 'NONE',  ( 43.01140435219951286, 79.12977050742732388, 38.86567161673127657 ) ) ;
#12916 = CARTESIAN_POINT ( 'NONE',  ( 47.43856463449117200, 139.7651871740939953, 32.77220824515698183 ) ) ;
#12917 = CARTESIAN_POINT ( 'NONE',  ( 38.01140435219951996, 93.56049967264873146, 32.58608133808903773 ) ) ;
#12918 = CARTESIAN_POINT ( 'NONE',  ( 67.39040179371399120, 143.9404232637865562, 4.720051584306741432 ) ) ;
#12919 = CARTESIAN_POINT ( 'NONE',  ( 38.04344971605643622, 95.40557500842271565, 34.86345644064632410 ) ) ;
#12920 = CARTESIAN_POINT ( 'NONE',  ( -143.3790856849358306, -159.6891397928654897, 43.77915905869157598 ) ) ;
#12921 = CARTESIAN_POINT ( 'NONE',  ( 38.58424406990784661, 90.26518717409398107, 35.64915139335016647 ) ) ;
#12922 = VECTOR ( 'NONE', #7617, 1000.000000000000000 ) ;
#12923 = CARTESIAN_POINT ( 'NONE',  ( 44.55648932407425633, 106.6104996726487428, 38.96596240072933170 ) ) ;
#12924 = CARTESIAN_POINT ( 'NONE',  ( 48.01140435219951996, 62.06049967264872436, 35.83527830041809636 ) ) ;
#12925 = ORIENTED_EDGE ( 'NONE', *, *, #17954, .T. ) ;
#12926 = CARTESIAN_POINT ( 'NONE',  ( 46.59305225739526435, 70.57977050742732672, 36.81289934271958941 ) ) ;
#12927 = CARTESIAN_POINT ( 'NONE',  ( -154.3824083646099439, -155.4938272943107052, 40.69124936498395328 ) ) ;
#12928 = ADVANCED_FACE ( 'NONE', ( #16131 ), #5375, .T. ) ;
#12929 = CARTESIAN_POINT ( 'NONE',  ( 40.02721236285810136, 85.80382532021769748, 0.4343372985580923329 ) ) ;
#12930 = CARTESIAN_POINT ( 'NONE',  ( -160.8964159109769696, -185.0084106276440821, 52.72008163687743121 ) ) ;
#12931 = ORIENTED_EDGE ( 'NONE', *, *, #13492, .T. ) ;
#12932 = DIRECTION ( 'NONE',  ( 0.000000000000000000, 0.000000000000000000, 1.000000000000000000 ) ) ;
#12933 = CARTESIAN_POINT ( 'NONE',  ( 42.21948215057684450, 105.4575765865522925, 39.21067981925355639 ) ) ;
#12934 =( BOUNDED_CURVE ( )  B_SPLINE_CURVE ( 1, ( #13717, #18794 ),
 .UNSPECIFIED., .F., .F. ) 
 B_SPLINE_CURVE_WITH_KNOTS ( ( 2, 2 ),
 ( 0.000000000000000000, 1.000000000000000000 ),
 .UNSPECIFIED. ) 
 CURVE ( )  GEOMETRIC_REPRESENTATION_ITEM ( )  RATIONAL_B_SPLINE_CURVE ( ( 0.9782074374858980015, 0.9782074374858980015 ) ) 
 REPRESENTATION_ITEM ( '' )  );
#12935 = VECTOR ( 'NONE', #20240, 1000.000000000000000 ) ;
#12936 = ORIENTED_EDGE ( 'NONE', *, *, #4121, .T. ) ;
#12937 = FILL_AREA_STYLE_COLOUR ( '', #11144 ) ;
#12938 = EDGE_LOOP ( 'NONE', ( #18209, #4547, #19015, #3009 ) ) ;
#12939 = CARTESIAN_POINT ( 'NONE',  ( 43.01140435219951286, 124.1297705074272955, 38.86567161673127657 ) ) ;
#12940 = AXIS2_PLACEMENT_3D ( 'NONE', #3180, #21704, #9909 ) ;
#12941 = CARTESIAN_POINT ( 'NONE',  ( -155.5590433672037705, -155.1145756620584564, 40.47124192889010885 ) ) ;
#12942 = CARTESIAN_POINT ( 'NONE',  ( 44.37947211624943833, 89.47977050742731819, 30.00020018409699318 ) ) ;
#12943 = CARTESIAN_POINT ( 'NONE',  ( 48.01140435219951996, 67.13445800887258486, 35.83527830041810347 ) ) ;
#12944 = DIRECTION ( 'NONE',  ( 0.000000000000000000, -1.000000000000000000, 0.000000000000000000 ) ) ;
#12945 = CARTESIAN_POINT ( 'NONE',  ( -176.9699209214867892, 482.8605407899846682, -19.99999999999995737 ) ) ;
#12946 = CARTESIAN_POINT ( 'NONE',  ( -151.4692556286853176, -175.7391397928654726, 59.65701158161632378 ) ) ;
#12947 = CARTESIAN_POINT ( 'NONE',  ( -154.5594255724347761, -190.8891397928654783, 59.16757674456785310 ) ) ;
#12948 = VECTOR ( 'NONE', #17367, 1000.000000000000000 ) ;
#12949 = DIRECTION ( 'NONE',  ( 1.000000000000000000, 0.000000000000000000, 0.000000000000000000 ) ) ;
#12950 = CARTESIAN_POINT ( 'NONE',  ( 43.80332655382220253, 94.95757658655229250, 29.21067981925356705 ) ) ;
#12951 = CARTESIAN_POINT ( 'NONE',  ( -143.8425227516148084, -186.0938272943107279, 44.11586579668791330 ) ) ;
#12952 = CARTESIAN_POINT ( 'NONE',  ( 47.05648932407426344, 123.9844580088725934, 37.14960608071593384 ) ) ;
#12953 = CARTESIAN_POINT ( 'NONE',  ( 47.43856463449117200, 106.7297705074273324, 35.64915139335016647 ) ) ;
#12954 = CARTESIAN_POINT ( 'NONE',  ( 16.41399813444308364, 129.5198218381110564, 15.55674365125313763 ) ) ;
#12955 = CARTESIAN_POINT ( 'NONE',  ( -145.6429501568359797, -183.8438272943107563, 57.67623309621198047 ) ) ;
#12956 = CARTESIAN_POINT ( 'NONE',  ( 47.43856463449117911, 94.76518717409399528, 32.77220824515697473 ) ) ;
#12957 = CARTESIAN_POINT ( 'NONE',  ( 18.67254549292281141, -61.68114226949890622, 30.00000000000000000 ) ) ;
#12958 = ORIENTED_EDGE ( 'NONE', *, *, #2399, .F. ) ;
#12959 = FACE_OUTER_BOUND ( 'NONE', #7525, .T. ) ;
#12960 = CARTESIAN_POINT ( 'NONE',  ( 26.13368487350976110, 90.12329638092472806, 0.9106621812756837686 ) ) ;
#12961 = CARTESIAN_POINT ( 'NONE',  ( 39.42975644700377558, 144.6797705074273495, 36.81289934271958941 ) ) ;
#12962 = CARTESIAN_POINT ( 'NONE',  ( 60.04598833032897431, 142.2798636455802921, -15.36278432740704147 ) ) ;
#12963 = ADVANCED_FACE ( 'NONE', ( #9426 ), #11986, .T. ) ;
#12964 = CARTESIAN_POINT ( 'NONE',  ( 47.43856463449117911, 71.02977050742730114, 32.77220824515697473 ) ) ;
#12965 = ORIENTED_EDGE ( 'NONE', *, *, #21126, .T. ) ;
#12966 = ORIENTED_EDGE ( 'NONE', *, *, #19622, .T. ) ;
#12967 = CARTESIAN_POINT ( 'NONE',  ( 41.64333658814960870, 155.7797705074273438, 30.00020018409699318 ) ) ;
#12968 = DIRECTION ( 'NONE',  ( -0.000000000000000000, -0.000000000000000000, -1.000000000000000000 ) ) ;
#12969 = CARTESIAN_POINT ( 'NONE',  ( 43.01140435219951286, 107.9604996726487371, 28.95336869806222779 ) ) ;
#12970 = CARTESIAN_POINT ( 'NONE',  ( 44.37947211624943833, 64.01518717409400949, 38.42115945441014446 ) ) ;
#12971 = CARTESIAN_POINT ( 'NONE',  ( 42.21948215057687293, 96.45757658655232092, 39.21067981925357060 ) ) ;
#12972 = CARTESIAN_POINT ( 'NONE',  ( -142.0420953463935803, -162.2438272943107336, 46.59394152635518083 ) ) ;
#12973 = CARTESIAN_POINT ( 'NONE',  ( -143.3790856849358306, -166.2891397928654840, 55.53486410454105027 ) ) ;
#12974 = CARTESIAN_POINT ( 'NONE',  ( -157.6495955161842062, -179.0130981290892578, 41.15050349809590102 ) ) ;
#12975 =( LENGTH_UNIT ( ) NAMED_UNIT ( * ) SI_UNIT ( .MILLI., .METRE. ) );
#12976 = CARTESIAN_POINT ( 'NONE',  ( 151.4773229304660731, 84.89323405393692212, 4.000000000000021316 ) ) ;
#12977 = EDGE_CURVE ( 'NONE', #8279, #18561, #10345, .T. ) ;
#12978 = CARTESIAN_POINT ( 'NONE',  ( 39.92123440845004723, 149.3344580088725877, 29.95742577749337343 ) ) ;
#12979 = CARTESIAN_POINT ( 'NONE',  ( 43.01140435219951286, 134.6297705074273097, 29.55568802177586463 ) ) ;
#12980 = CARTESIAN_POINT ( 'NONE',  ( 9.691656460246418803, 128.1079710775123601, 15.35877872671195910 ) ) ;
#12981 = CARTESIAN_POINT ( 'NONE',  ( 45.74753988029934249, 131.0651871740940067, 30.44471234641812174 ) ) ;
#12982 = CARTESIAN_POINT ( 'NONE',  ( -154.5594255724347761, -166.8891397928654499, 59.16757674456785310 ) ) ;
#12983 = DIRECTION ( 'NONE',  ( 0.000000000000000000, 1.000000000000000000, 0.000000000000000000 ) ) ;
#12984 = EDGE_CURVE ( 'NONE', #15219, #1195, #15452, .T. ) ;
#12985 = LINE ( 'NONE', #6140, #14703 ) ;
#12986 = DIRECTION ( 'NONE',  ( -1.000000000000000000, 0.000000000000000000, 0.000000000000000000 ) ) ;
#12987 = EDGE_CURVE ( 'NONE', #9753, #1056, #5029, .T. ) ;
#12988 = CARTESIAN_POINT ( 'NONE',  ( 14.76087776054169787, 121.2312262212812755, 22.22355758277721804 ) ) ;
#12989 = CARTESIAN_POINT ( 'NONE',  ( 48.01140435219951996, 83.21049967264873715, 34.21067981925357060 ) ) ;
#12990 = VECTOR ( 'NONE', #7906, 1000.000000000000114 ) ;
#12991 = VERTEX_POINT ( 'NONE', #11612 ) ;
#12992 = EDGE_CURVE ( 'NONE', #9338, #8983, #9536, .T. ) ;
#12993 = CARTESIAN_POINT ( 'NONE',  ( -148.3790856849358306, -156.3891397928654783, 40.14644641866477315 ) ) ;
#12994 = ORIENTED_EDGE ( 'NONE', *, *, #1961, .F. ) ;
#12995 = CARTESIAN_POINT ( 'NONE',  ( 38.96631938032478359, 80.48445800887257917, 31.27175355779120025 ) ) ;
#12996 = FACE_OUTER_BOUND ( 'NONE', #15928, .T. ) ;
#12997 = CARTESIAN_POINT ( 'NONE',  ( 39.92123440845004723, 138.2604996726487059, 29.95742577749337343 ) ) ;
#12999 = CARTESIAN_POINT ( 'NONE',  ( 51.06471579629997137, 92.96554497763615643, 8.089385107838625188 ) ) ;
#12998 = CARTESIAN_POINT ( 'NONE',  ( 39.42975644700377558, 95.81518717409399244, 31.60846029578754468 ) ) ;
#13000 = CARTESIAN_POINT ( 'NONE',  ( -157.2955611005346270, -170.6084106276440480, 41.63779006702063867 ) ) ;
#13001 = CARTESIAN_POINT ( 'NONE',  ( 38.96631938032478359, 67.01049967264874851, 37.14960608071593384 ) ) ;
#13003 = DIRECTION ( 'NONE',  ( -0.000000000000000000, -0.000000000000000000, -1.000000000000000000 ) ) ;
#13002 = CARTESIAN_POINT ( 'NONE',  ( -151.4692556286853176, -179.3130981290892976, 39.65701158161629536 ) ) ;
#13004 = CARTESIAN_POINT ( 'NONE',  ( 43.01140435219951286, 65.96049967264873715, 29.21067981925356705 ) ) ;
#13005 = VECTOR ( 'NONE', #14259, 1000.000000000000000 ) ;
#13006 = CARTESIAN_POINT ( 'NONE',  ( -151.4692556286852891, -188.3130981290893260, 39.65701158161629536 ) ) ;
#13007 = CARTESIAN_POINT ( 'NONE',  ( 44.55648932407425633, 115.8844580088725991, 29.45539723777780239 ) ) ;
#13008 = CARTESIAN_POINT ( 'NONE',  ( 46.59305225739526435, 64.91518717409400097, 31.60846029578754468 ) ) ;
#13009 = CARTESIAN_POINT ( 'NONE',  ( 75.10802748102119608, 108.0013139708956800, -8.018167963582932600 ) ) ;
#13010 = CARTESIAN_POINT ( 'NONE',  ( 18.67254549292281496, -61.68114226949890622, 10.00000000000001599 ) ) ;
#13011 = CARTESIAN_POINT ( 'NONE',  ( -151.4692556286852891, -169.1438272943107108, 59.56931450028537967 ) ) ;
#13012 = CARTESIAN_POINT ( 'NONE',  ( -154.3824083646099439, -187.5584106276440650, 58.62277379824867296 ) ) ;
#13013 = ADVANCED_FACE ( 'NONE', ( #14582 ), #4670, .T. ) ;
#13014 = ORIENTED_EDGE ( 'NONE', *, *, #5195, .F. ) ;
#13015 = CARTESIAN_POINT ( 'NONE',  ( 38.58424406990785371, 71.96518717409399812, 32.77220824515697473 ) ) ;
#13016 = CARTESIAN_POINT ( 'NONE',  ( -145.6429501568359797, -172.1084106276439911, 57.67623309621198047 ) ) ;
#13017 = CARTESIAN_POINT ( 'NONE',  ( 9.157865646370469292, 114.3054763464604662, 21.90616645148510599 ) ) ;
#13018 = PRESENTATION_STYLE_ASSIGNMENT (( #1113 ) ) ;
#13019 = CARTESIAN_POINT ( 'NONE',  ( 44.37947211624943833, 134.2151871740940123, 30.00020018409699318 ) ) ;
#13020 = CARTESIAN_POINT ( 'NONE',  ( 64.37283757718545019, 93.25908544850187809, -13.41832554473225692 ) ) ;
#13021 = ORIENTED_EDGE ( 'NONE', *, *, #8338, .T. ) ;
#13022 = VERTEX_POINT ( 'NONE', #16452 ) ;
#13023 = FACE_OUTER_BOUND ( 'NONE', #395, .T. ) ;
#13024 = CARTESIAN_POINT ( 'NONE',  ( 15.66613903973849986, 126.7949701480144711, 9.441967288829692606 ) ) ;
#13025 = ORIENTED_EDGE ( 'NONE', *, *, #7470, .T. ) ;
#13026 = CARTESIAN_POINT ( 'NONE',  ( 46.10157429594899270, 116.6604996726487258, 29.95742577749336988 ) ) ;
#13028 = CARTESIAN_POINT ( 'NONE',  ( 44.86974823489592978, 148.0457227541334362, 10.98970740178311090 ) ) ;
#13027 = CARTESIAN_POINT ( 'NONE',  ( 47.43856463449117200, 127.4651871740940123, 35.64915139335016647 ) ) ;
#13029 = CARTESIAN_POINT ( 'NONE',  ( 43.01140435219951286, 95.96049967264876557, 28.95336869806222779 ) ) ;
#13030 = PLANE ( 'NONE',  #11827 ) ;
#13031 = DIRECTION ( 'NONE',  ( 0.000000000000000000, 1.000000000000000000, 0.000000000000000000 ) ) ;
#13032 = CARTESIAN_POINT ( 'NONE',  ( -161.4692556286852607, -158.6391397928654783, 46.40781461928724383 ) ) ;
#13033 = CARTESIAN_POINT ( 'NONE',  ( 41.64333658814960870, 90.71518717409401233, 38.42115945441014446 ) ) ;
#13034 = CARTESIAN_POINT ( 'NONE',  ( 44.55648932407425633, 150.6844580088725820, 38.96596240072933170 ) ) ;
#13035 = CARTESIAN_POINT ( 'NONE',  ( 47.05648932407426344, 71.51049967264873430, 31.27175355779120025 ) ) ;
#13036 = CARTESIAN_POINT ( 'NONE',  ( -151.4692556286852891, -196.9891397928655010, 59.65701158161632378 ) ) ;
#13037 = ORIENTED_EDGE ( 'NONE', *, *, #2773, .T. ) ;
#13038 = CARTESIAN_POINT ( 'NONE',  ( 46.59305225739526435, 79.57977050742731251, 36.81289934271958941 ) ) ;
#13039 = CARTESIAN_POINT ( 'NONE',  ( -151.4692556286852891, -194.9084106276440025, 39.74470866294723947 ) ) ;
#13040 = CARTESIAN_POINT ( 'NONE',  ( 8.798315742295939046, 121.0924013121165075, 9.124689178586496752 ) ) ;
#13041 = CARTESIAN_POINT ( 'NONE',  ( -160.8964159109769696, -182.1584106276440309, 49.65701158161630957 ) ) ;
#13042 = ORIENTED_EDGE ( 'NONE', *, *, #2304, .T. ) ;
#13043 = FACE_BOUND ( 'NONE', #18393, .T. ) ;
#13044 = CARTESIAN_POINT ( 'NONE',  ( -145.2889157411863437, -159.5391397928654555, 41.15050349809589392 ) ) ;
#13045 = CARTESIAN_POINT ( 'NONE',  ( 41.64333658814960870, 123.9797705074273324, 38.42115945441014446 ) ) ;
#13046 = VERTEX_POINT ( 'NONE', #12827 ) ;
#13047 = DIRECTION ( 'NONE',  ( -0.000000000000000000, 1.000000000000000000, -0.000000000000000000 ) ) ;
#13048 = EDGE_LOOP ( 'NONE', ( #12665, #9286, #1333, #14693 ) ) ;
#13049 = CARTESIAN_POINT ( 'NONE',  ( 38.58424406990784661, 120.2297705074273182, 32.77220824515698183 ) ) ;
#13050 = CARTESIAN_POINT ( 'NONE',  ( 43.80332655382220253, 58.95757658655231381, 29.21067981925356705 ) ) ;
#13051 = CARTESIAN_POINT ( 'NONE',  ( 43.01140435219951286, 66.53445800887256212, 39.46799094044489209 ) ) ;
#13052 = EDGE_CURVE ( 'NONE', #5698, #8850, #11771, .T. ) ;
#13053 = CARTESIAN_POINT ( 'NONE',  ( 43.01140435219954838, 131.0344580088725479, 29.21067981925356705 ) ) ;
#13054 = DIRECTION ( 'NONE',  ( 0.000000000000000000, 0.000000000000000000, 1.000000000000000000 ) ) ;
#13055 = PRESENTATION_STYLE_ASSIGNMENT (( #19448 ) ) ;
#13056 = CARTESIAN_POINT ( 'NONE',  ( -161.4692556286853176, -188.4891397928654726, 49.65701158161630957 ) ) ;
#13057 = CARTESIAN_POINT ( 'NONE',  ( 43.01140435219951996, 155.9604996726487514, 29.21067981925357060 ) ) ;
#13058 = CARTESIAN_POINT ( 'NONE',  ( 39.92123440845005433, 102.2604996726487485, 29.95742577749336988 ) ) ;
#13059 = CARTESIAN_POINT ( 'NONE',  ( -160.8964159109769696, -191.0438272943107449, 46.59394152635518793 ) ) ;
#13060 = CARTESIAN_POINT ( 'NONE',  ( 48.01140435219951996, 121.2844580088725763, 34.21067981925357060 ) ) ;
#13061 = CARTESIAN_POINT ( 'NONE',  ( 38.58424406990786082, 102.3797705074273381, 34.21067981925357060 ) ) ;
#13062 =( BOUNDED_CURVE ( )  B_SPLINE_CURVE ( 2, ( #8929, #12441, #12550, #10797, #9255, #17500, #2411, #20718, #12110, #331, #13980, #7060, #18842 ),
 .UNSPECIFIED., .F., .F. ) 
 B_SPLINE_CURVE_WITH_KNOTS ( ( 3, 2, 2, 2, 2, 2, 3 ),
 ( 0.6544117647058823595, 0.6558823529411764719, 0.6588235294117646967, 0.6617647058823529216, 0.6647058823529411464, 0.6676470588235293713, 0.6691176470588234837 ),
 .UNSPECIFIED. ) 
 CURVE ( )  GEOMETRIC_REPRESENTATION_ITEM ( )  RATIONAL_B_SPLINE_CURVE ( ( 0.9755282581475768211, 0.9755282581475768211, 1.000000000000000000, 0.9510565162951535312, 1.000000000000000000, 0.9510565162951535312, 1.000000000000000000, 0.9510565162951535312, 1.000000000000000000, 0.9510565162951535312, 1.000000000000000000, 0.9755282581475768211, 0.9755282581475768211 ) ) 
 REPRESENTATION_ITEM ( '' )  );
#13063 = CARTESIAN_POINT ( 'NONE',  ( 27.44638778410068625, 143.5188605762539851, 16.27111261720311930 ) ) ;
#13064 = CARTESIAN_POINT ( 'NONE',  ( -142.0420953463936087, -180.3938272943107108, 49.65701158161630957 ) ) ;
#13065 = CARTESIAN_POINT ( 'NONE',  ( 44.37947211624943833, 86.21518717409399812, 30.00020018409699318 ) ) ;
#13066 = DIRECTION ( 'NONE',  ( 0.000000000000000000, 1.000000000000000000, 0.000000000000000000 ) ) ;
#13067 = ORIENTED_EDGE ( 'NONE', *, *, #8693, .T. ) ;
#13068 = DIRECTION ( 'NONE',  ( 1.140132994654635861E-16, 0.000000000000000000, 1.000000000000000000 ) ) ;
#13069 = CARTESIAN_POINT ( 'NONE',  ( 24.41145734808947054, 148.6458414325078081, 10.19629000755267434 ) ) ;
#13070 = CARTESIAN_POINT ( 'NONE',  ( 15.04800518778627882, 122.8738276488686694, -10.72018599084894319 ) ) ;
#13071 = EDGE_CURVE ( 'NONE', #15098, #15220, #11387, .T. ) ;
#13072 = CARTESIAN_POINT ( 'NONE',  ( 39.42975644700377558, 63.07977050742731251, 31.60846029578754468 ) ) ;
#13073 = ORIENTED_EDGE ( 'NONE', *, *, #21212, .F. ) ;
#13074 = EDGE_LOOP ( 'NONE', ( #18094, #19126, #20778, #15567 ) ) ;
#13075 = CARTESIAN_POINT ( 'NONE',  ( 46.59305225739526435, 152.1797705074273210, 31.60846029578754468 ) ) ;
#13076 = FACE_OUTER_BOUND ( 'NONE', #15614, .T. ) ;
#13077 = CARTESIAN_POINT ( 'NONE',  ( 39.92123440845004723, 112.1604996726487258, 38.46393386101376421 ) ) ;
#13078 = CARTESIAN_POINT ( 'NONE',  ( 46.59305225739526435, 67.31518717409400665, 36.81289934271958941 ) ) ;
#13079 = DIRECTION ( 'NONE',  ( 0.000000000000000000, 0.000000000000000000, 1.000000000000000000 ) ) ;
#13080 = CARTESIAN_POINT ( 'NONE',  ( -145.6429501568359797, -159.8438272943107279, 57.67623309621197336 ) ) ;
#13081 = DIRECTION ( 'NONE',  ( 0.000000000000000000, 1.000000000000000000, 0.000000000000000000 ) ) ;
#13082 = CARTESIAN_POINT ( 'NONE',  ( -151.4692556286852891, -176.3130981290892692, 39.14238933923362396 ) ) ;
#13083 = FACE_OUTER_BOUND ( 'NONE', #9043, .T. ) ;
#13085 = EDGE_CURVE ( 'NONE', #2592, #20857, #7882, .T. ) ;
#13084 = CARTESIAN_POINT ( 'NONE',  ( 41.46631938032478359, 150.3844580088725991, 38.96596240072933170 ) ) ;
#13086 = CARTESIAN_POINT ( 'NONE',  ( 39.42975644700377558, 129.6797705074273210, 36.81289934271958941 ) ) ;
#13087 = CARTESIAN_POINT ( 'NONE',  ( 66.46241511549931147, 94.85692098654722315, 12.50163586956050210 ) ) ;
#13088 = CARTESIAN_POINT ( 'NONE',  ( 38.58424406990786082, 114.1151871740939896, 34.21067981925357060 ) ) ;
#13089 = LINE ( 'NONE', #3058, #19933 ) ;
#13090 = VECTOR ( 'NONE', #2037, 1000.000000000000000 ) ;
#13091 = CARTESIAN_POINT ( 'NONE',  ( 39.92123440845005433, 150.2604996726487911, 29.95742577749336988 ) ) ;
#13093 = CARTESIAN_POINT ( 'NONE',  ( 43.01140435219951996, 10.71049967264875491, 29.21067981925357060 ) ) ;
#13092 = VECTOR ( 'NONE', #5321, 1000.000000000000114 ) ;
#13094 = PLANE ( 'NONE',  #4286 ) ;
#13095 = CARTESIAN_POINT ( 'NONE',  ( 61.21858502650649569, 141.5469622553929128, 17.69968404581608823 ) ) ;
#13096 = CARTESIAN_POINT ( 'NONE',  ( 39.92123440845005433, 120.2604996726487485, 29.95742577749336988 ) ) ;
#13097 = VECTOR ( 'NONE', #16028, 1000.000000000000000 ) ;
#13098 = EDGE_LOOP ( 'NONE', ( #6578, #2456 ) ) ;
#13099 = EDGE_CURVE ( 'NONE', #11964, #9411, #390, .T. ) ;
#13100 = CARTESIAN_POINT ( 'NONE',  ( -149.8854112254399240, -167.3899795514095672, 39.65701158161629536 ) ) ;
#13101 = ORIENTED_EDGE ( 'NONE', *, *, #7205, .F. ) ;
#13102 = CARTESIAN_POINT ( 'NONE',  ( 44.55648932407425633, 79.88445800887257064, 29.45539723777780239 ) ) ;
#13103 = CARTESIAN_POINT ( 'NONE',  ( 47.05648932407426344, 103.5844580088725877, 31.27175355779120025 ) ) ;
#13104 = AXIS2_PLACEMENT_3D ( 'NONE', #19174, #10695, #12555 ) ;
#13105 = CARTESIAN_POINT ( 'NONE',  ( 43.01140435219951286, 136.4604996726487229, 39.46799094044489209 ) ) ;
#13107 = CARTESIAN_POINT ( 'NONE',  ( 15.21076168709227616, 115.6846582791190201, 9.994193321846964295 ) ) ;
#13106 = CARTESIAN_POINT ( 'NONE',  ( 47.43856463449117200, 100.4651871740939839, 35.64915139335016647 ) ) ;
#13108 = CARTESIAN_POINT ( 'NONE',  ( 137.5268905834513191, 193.0332408774651185, -50.99999999999998579 ) ) ;
#13109 = ADVANCED_FACE ( 'NONE', ( #4556 ), #14910, .F. ) ;
#13110 = CARTESIAN_POINT ( 'NONE',  ( -159.0959885057557983, -167.4584106276440423, 44.11586579668791330 ) ) ;
#13111 = CARTESIAN_POINT ( 'NONE',  ( -151.4692556286852891, -191.6438272943107108, 39.74470866294723947 ) ) ;
#13113 = CARTESIAN_POINT ( 'NONE',  ( 43.80332655382220253, 69.61133943119284595, 39.21067981925355639 ) ) ;
#13112 = CARTESIAN_POINT ( 'NONE',  ( -46.09493621325655255, 160.7104996726487229, -25.00000000000000000 ) ) ;
#13114 = CARTESIAN_POINT ( 'NONE',  ( 43.01140435219951286, 143.0344580088726048, 29.21067981925356705 ) ) ;
#13115 = CARTESIAN_POINT ( 'NONE',  ( -151.4692556286853176, -174.2391397928654726, 39.65701158161629536 ) ) ;
#13116 = CARTESIAN_POINT ( 'NONE',  ( 44.37947211624943833, 59.21518717409400523, 30.00020018409699318 ) ) ;
#13117 = CARTESIAN_POINT ( 'NONE',  ( -154.5594255724347761, -183.9630981290893033, 59.16757674456785310 ) ) ;
#13118 = CARTESIAN_POINT ( 'NONE',  ( 30.24639091383375700, 151.6717570033048048, 3.410403464249057492 ) ) ;
#13119 = CARTESIAN_POINT ( 'NONE',  ( 43.01140435219951286, 152.3651871740939896, 29.55568802177586107 ) ) ;
#13120 = CARTESIAN_POINT ( 'NONE',  ( -148.5561028927606344, -158.7938272943107449, 40.69124936498395328 ) ) ;
#13121 = CARTESIAN_POINT ( 'NONE',  ( -160.8964159109769696, -182.0084106276440536, 52.72008163687743121 ) ) ;
#13122 = VERTEX_POINT ( 'NONE', #7990 ) ;
#13123 = CARTESIAN_POINT ( 'NONE',  ( 41.64333658814960870, 69.71518717409399812, 38.42115945441014446 ) ) ;
#13124 = CARTESIAN_POINT ( 'NONE',  ( -143.8425227516148084, -171.9584106276440423, 55.19815736654470584 ) ) ;
#13125 = CARTESIAN_POINT ( 'NONE',  ( 73.16288888369128074, 103.5245705370889766, 12.14422718744263285 ) ) ;
#13126 = PLANE ( 'NONE',  #10 ) ;
#13127 = CARTESIAN_POINT ( 'NONE',  ( 43.01140435219951286, 128.3651871740940180, 29.55568802177586463 ) ) ;
#13128 = CARTESIAN_POINT ( 'NONE',  ( 21.10625685842435928, 146.1099207202125854, -2.942173209646314014 ) ) ;
#13129 = ORIENTED_EDGE ( 'NONE', *, *, #4244, .F. ) ;
#13130 = CARTESIAN_POINT ( 'NONE',  ( 22.52008984372607614, 139.2495111981779985, 17.01435058386764965 ) ) ;
#13131 = ORIENTED_EDGE ( 'NONE', *, *, #1914, .T. ) ;
#13132 = CARTESIAN_POINT ( 'NONE',  ( 47.05648932407426344, 108.9844580088725792, 37.14960608071593384 ) ) ;
#13133 = FACE_OUTER_BOUND ( 'NONE', #16787, .T. ) ;
#13134 = CARTESIAN_POINT ( 'NONE',  ( 40.27526882409969033, 62.92977050742729972, 30.44471234641811819 ) ) ;
#13136 = CARTESIAN_POINT ( 'NONE',  ( 14.88799800344823154, 117.8296896831652560, 9.085076399755989129 ) ) ;
#13135 = CARTESIAN_POINT ( 'NONE',  ( 38.58424406990784661, 123.2651871740939953, 35.64915139335016647 ) ) ;
#13137 = CARTESIAN_POINT ( 'NONE',  ( 48.01140435219951996, 80.36049967264874283, 32.58608133808903773 ) ) ;
#13138 = CYLINDRICAL_SURFACE ( 'NONE', #19917, 7.500000000000007105 ) ;
#13139 = DIRECTION ( 'NONE',  ( 0.000000000000000000, 0.000000000000000000, 1.000000000000000000 ) ) ;
#13140 = CARTESIAN_POINT ( 'NONE',  ( 39.92123440845005433, 139.1604996726487400, 38.46393386101375711 ) ) ;
#13141 = CARTESIAN_POINT ( 'NONE',  ( 45.74753988029933538, 88.16518717409397254, 37.97664729208901946 ) ) ;
#13142 = DIRECTION ( 'NONE',  ( 0.000000000000000000, 0.000000000000000000, 1.000000000000000000 ) ) ;
#13143 = CARTESIAN_POINT ( 'NONE',  ( 48.01140435219951996, 142.4344580088725820, 32.58608133808903773 ) ) ;
#13144 = ORIENTED_EDGE ( 'NONE', *, *, #20373, .T. ) ;
#13145 = CARTESIAN_POINT ( 'NONE',  ( 38.58424406990786082, 66.37977050742730967, 34.21067981925357060 ) ) ;
#13146 = CARTESIAN_POINT ( 'NONE',  ( -160.8964159109769696, -157.7438272943107336, 52.72008163687743121 ) ) ;
#13147 = CARTESIAN_POINT ( 'NONE',  ( 11.67247064774405452, 106.1322524520788875, 1.624861436118421043 ) ) ;
#13148 = CARTESIAN_POINT ( 'NONE',  ( -157.2955611005346270, -185.6084106276440195, 41.63779006702063867 ) ) ;
#13149 = EDGE_LOOP ( 'NONE', ( #361, #9313, #12936, #1548 ) ) ;
#13150 = CARTESIAN_POINT ( 'NONE',  ( 173.3794444120442506, -136.9891397928655010, 67.64809332337412684 ) ) ;
#13151 = CARTESIAN_POINT ( 'NONE',  ( -151.4692556286852607, -159.2391397928654726, 39.65701158161629536 ) ) ;
#13152 = CARTESIAN_POINT ( 'NONE',  ( 40.27526882409969744, 126.8297705074273125, 37.97664729208901235 ) ) ;
#13153 = CARTESIAN_POINT ( 'NONE',  ( 57.94507594753278568, 150.7106492751291569, -2.660852849641732298 ) ) ;
#13154 = VERTEX_POINT ( 'NONE', #4777 ) ;
#13155 = EDGE_CURVE ( 'NONE', #4775, #7018, #16561, .T. ) ;
#13156 = ADVANCED_FACE ( 'NONE', ( #16346 ), #20009, .F. ) ;
#13157 = CARTESIAN_POINT ( 'NONE',  ( 48.01140435219951996, 88.13445800887258486, 35.83527830041809636 ) ) ;
#13158 = ORIENTED_EDGE ( 'NONE', *, *, #6789, .T. ) ;
#13159 = CARTESIAN_POINT ( 'NONE',  ( 47.43856463449117200, 119.0297705074273296, 32.77220824515698183 ) ) ;
#13160 = CARTESIAN_POINT ( 'NONE',  ( 42.21948215057687293, 72.03738109496900677, 29.21067981925355994 ) ) ;
#13161 = CARTESIAN_POINT ( 'NONE',  ( 45.74753988029933538, 155.0651871740940067, 30.44471234641811819 ) ) ;
#13162 = CARTESIAN_POINT ( 'NONE',  ( -158.9748091281504401, -126.9891397928655010, 62.65701158161630957 ) ) ;
#13163 = CARTESIAN_POINT ( 'NONE',  ( -59.65946286876558702, 788.4655180356369328, -19.99999999999997868 ) ) ;
#13164 = CARTESIAN_POINT ( 'NONE',  ( -145.2889157411863721, -177.5391397928654840, 41.15050349809590102 ) ) ;
#13165 = CARTESIAN_POINT ( 'NONE',  ( 83.67254549292280785, -61.68114226949890622, 20.00000000000001776 ) ) ;
#13166 = DIRECTION ( 'NONE',  ( -1.000000000000000000, 0.000000000000000000, 0.000000000000000000 ) ) ;
#13167 = CARTESIAN_POINT ( 'NONE',  ( -145.6429501568359797, -185.9438272943107506, 41.63779006702063867 ) ) ;
#13168 = CONTEXT_DEPENDENT_SHAPE_REPRESENTATION ( #9723, #11521 ) ;
#13169 = CARTESIAN_POINT ( 'NONE',  ( 48.01140435219951996, 124.1344580088725706, 35.83527830041810347 ) ) ;
#13170 = CARTESIAN_POINT ( 'NONE',  ( 40.27526882409969033, 107.9297705074273352, 30.44471234641811819 ) ) ;
#13171 = CARTESIAN_POINT ( 'NONE',  ( 31.34884810169724645, 145.5825485123889109, -10.55804779818428862 ) ) ;
#13172 = CARTESIAN_POINT ( 'NONE',  ( -157.2955611005346270, -184.4438272943107506, 57.67623309621198047 ) ) ;
#13173 = AXIS2_PLACEMENT_3D ( 'NONE', #18457, #10083, #11837 ) ;
#13174 = CARTESIAN_POINT ( 'NONE',  ( 40.27526882409969744, 84.56518717409399244, 37.97664729208901235 ) ) ;
#13175 = CARTESIAN_POINT ( 'NONE',  ( 26.17254549292281496, -61.68114226949890622, 20.00000000000001776 ) ) ;
#13176 = ORIENTED_EDGE ( 'NONE', *, *, #8525, .F. ) ;
#13177 = CARTESIAN_POINT ( 'NONE',  ( 47.05648932407426344, 128.5104996726487343, 31.27175355779120025 ) ) ;
#13178 = DIRECTION ( 'NONE',  ( -0.000000000000000000, -0.000000000000000000, -1.000000000000000000 ) ) ;
#13179 = CARTESIAN_POINT ( 'NONE',  ( 28.97945247615869846, 95.53788343559241980, -5.005900276531492388 ) ) ;
#13180 = CARTESIAN_POINT ( 'NONE',  ( 46.59305225739526435, 70.57977050742732672, 36.81289934271958941 ) ) ;
#13181 = ORIENTED_EDGE ( 'NONE', *, *, #17540, .F. ) ;
#13182 = CARTESIAN_POINT ( 'NONE',  ( 41.64333658814960870, 144.9797705074273324, 38.42115945441014446 ) ) ;
#13183 = LINE ( 'NONE', #11199, #16866 ) ;
#13184 = AXIS2_PLACEMENT_3D ( 'NONE', #10874, #20898, #11259 ) ;
#13185 = CARTESIAN_POINT ( 'NONE',  ( 47.05648932407426344, 107.5104996726487485, 31.27175355779120025 ) ) ;
#13186 = CARTESIAN_POINT ( 'NONE',  ( 43.01140435219951286, 68.36518717409400381, 29.55568802177586463 ) ) ;
#13187 = CARTESIAN_POINT ( 'NONE',  ( -143.8425227516148084, -156.3584106276440480, 44.11586579668791330 ) ) ;
#13188 =( BOUNDED_CURVE ( )  B_SPLINE_CURVE ( 2, ( #927, #9105, #7672, #15415, #19443, #6934, #19232, #14371, #716, #20375, #13746, #20999, #18822 ),
 .UNSPECIFIED., .F., .F. ) 
 B_SPLINE_CURVE_WITH_KNOTS ( ( 3, 2, 2, 2, 2, 2, 3 ),
 ( 0.2426470588235294101, 0.2441176470588235226, 0.2470588235294117752, 0.2500000000000000000, 0.2529411764705882248, 0.2558823529411764497, 0.2573529411764705621 ),
 .UNSPECIFIED. ) 
 CURVE ( )  GEOMETRIC_REPRESENTATION_ITEM ( )  RATIONAL_B_SPLINE_CURVE ( ( 0.9755282581475768211, 0.9755282581475768211, 1.000000000000000000, 0.9510565162951535312, 1.000000000000000000, 0.9510565162951535312, 1.000000000000000000, 0.9510565162951535312, 1.000000000000000000, 0.9510565162951535312, 1.000000000000000000, 0.9755282581475772652, 0.9755282581475768211 ) ) 
 REPRESENTATION_ITEM ( '' )  );
#13189 = CARTESIAN_POINT ( 'NONE',  ( -148.5561028927606344, -161.7938272943107449, 40.69124936498395328 ) ) ;
#13190 = CARTESIAN_POINT ( 'NONE',  ( -151.4692556286852607, -166.7391397928654158, 59.65701158161632378 ) ) ;
#13191 = CARTESIAN_POINT ( 'NONE',  ( -148.3790856849358306, -174.6630981290893203, 59.16757674456786020 ) ) ;
#13192 = CARTESIAN_POINT ( 'NONE',  ( 11.17254549292281673, -61.68114226949890622, 10.00000000000001599 ) ) ;
#13193 = CARTESIAN_POINT ( 'NONE',  ( 39.92123440845004723, 150.2344580088725365, 38.46393386101376421 ) ) ;
#13194 = CARTESIAN_POINT ( 'NONE',  ( 47.43856463449117200, 137.0297705074272869, 32.77220824515698183 ) ) ;
#13195 = CARTESIAN_POINT ( 'NONE',  ( 21.21153947156776809, 146.4065673692475400, 16.07276909216647454 ) ) ;
#13196 = CARTESIAN_POINT ( 'NONE',  ( 41.64333658814960870, 116.5151871740940095, 30.00020018409699318 ) ) ;
#13197 = CARTESIAN_POINT ( 'NONE',  ( -159.5594255724347761, -182.1891397928654612, 55.53486410454104316 ) ) ;
#13198 = DIRECTION ( 'NONE',  ( -0.000000000000000000, 0.000000000000000000, 1.000000000000000000 ) ) ;
#13199 = CARTESIAN_POINT ( 'NONE',  ( 48.01140435219951996, 65.21049967264873715, 34.21067981925357060 ) ) ;
#13200 = CARTESIAN_POINT ( 'NONE',  ( 65.38231449488820601, 145.7134111962467671, 5.629255361809699210 ) ) ;
#13201 = CARTESIAN_POINT ( 'NONE',  ( 30.88693878601983300, 94.35661743609990992, 20.91413290821214588 ) ) ;
#13202 = CARTESIAN_POINT ( 'NONE',  ( -145.2889157411863437, -186.5391397928654271, 41.15050349809589392 ) ) ;
#13203 = CARTESIAN_POINT ( 'NONE',  ( 43.01140435219951286, 100.1297705074273239, 38.86567161673127657 ) ) ;
#13204 = ORIENTED_EDGE ( 'NONE', *, *, #12987, .F. ) ;
#13205 = VECTOR ( 'NONE', #18917, 1000.000000000000000 ) ;
#13206 = CARTESIAN_POINT ( 'NONE',  ( -151.4692556286852607, -167.3130981290893260, 39.65701158161629536 ) ) ;
#13207 = VERTEX_POINT ( 'NONE', #6323 ) ;
#13208 = CARTESIAN_POINT ( 'NONE',  ( 39.92123440845004723, 78.23445800887257917, 38.46393386101376421 ) ) ;
#13209 = DIRECTION ( 'NONE',  ( -0.3450121214752275289, 0.9385982292947088190, 0.000000000000000000 ) ) ;
#13210 = CARTESIAN_POINT ( 'NONE',  ( 48.01140435219951996, 143.2104996726487514, 34.21067981925357060 ) ) ;
#13212 = CARTESIAN_POINT ( 'NONE',  ( 42.05360093099289287, 148.0107091728485500, 4.874927614337289938 ) ) ;
#13211 = CARTESIAN_POINT ( 'NONE',  ( 41.64333658814960870, 96.71518717409399812, 38.42115945441014446 ) ) ;
#13213 = DIRECTION ( 'NONE',  ( -0.3450121214752274734, 0.9385982292947088190, 0.000000000000000000 ) ) ;
#13214 = CARTESIAN_POINT ( 'NONE',  ( -154.3824083646099439, -169.5584106276440366, 58.62277379824867296 ) ) ;
#13215 = CARTESIAN_POINT ( 'NONE',  ( -154.3824083646099439, -187.2938272943107449, 58.62277379824867296 ) ) ;
#13217 = CARTESIAN_POINT ( 'NONE',  ( 46.10157429594899270, 70.73445800887257917, 29.95742577749336988 ) ) ;
#13216 = DIRECTION ( 'NONE',  ( -0.3450121214752274734, 0.9385982292947088190, 0.000000000000000000 ) ) ;
#13218 = CARTESIAN_POINT ( 'NONE',  ( 151.4773229304660731, 84.89323405393692212, 14.00000000000001776 ) ) ;
#13219 = CARTESIAN_POINT ( 'NONE',  ( 38.01140435219952707, 147.7104996726487514, 34.21067981925357060 ) ) ;
#13220 = CARTESIAN_POINT ( 'NONE',  ( 121.4021762516569964, 137.5714195593754710, 4.000000000000003553 ) ) ;
#13221 = EDGE_CURVE ( 'NONE', #3828, #12910, #16763, .T. ) ;
#13222 = CARTESIAN_POINT ( 'NONE',  ( 43.01140435219951286, 59.36518717409399670, 29.55568802177586463 ) ) ;
#13223 = DIRECTION ( 'NONE',  ( -0.000000000000000000, -0.000000000000000000, -1.000000000000000000 ) ) ;
#13224 = CARTESIAN_POINT ( 'NONE',  ( 76.92284642892752800, 124.5854180935290714, 5.434424407683230207 ) ) ;
#13225 = CARTESIAN_POINT ( 'NONE',  ( 39.42975644700377558, 149.8151871740940067, 31.60846029578754468 ) ) ;
#13226 = VECTOR ( 'NONE', #13598, 1000.000000000000000 ) ;
#13227 = CARTESIAN_POINT ( 'NONE',  ( -157.2955611005346270, -157.4438272943107506, 57.67623309621198047 ) ) ;
#13228 = CARTESIAN_POINT ( 'NONE',  ( -157.2955611005345986, -172.7084106276440423, 57.67623309621197336 ) ) ;
#13229 = VERTEX_POINT ( 'NONE', #3242 ) ;
#13230 = CARTESIAN_POINT ( 'NONE',  ( 38.01140435219952707, 77.93445800887255359, 35.83527830041809636 ) ) ;
#13231 = CARTESIAN_POINT ( 'NONE',  ( -160.8964159109769696, -158.1584106276440593, 49.65701158161630957 ) ) ;
#13232 = CARTESIAN_POINT ( 'NONE',  ( 38.74908582987571748, 85.85911260889788821, 20.47761041045779606 ) ) ;
#13233 = CARTESIAN_POINT ( 'NONE',  ( 46.10157429594899270, 112.7344580088725792, 29.95742577749336988 ) ) ;
#13234 = CARTESIAN_POINT ( 'NONE',  ( 38.58424406990784661, 123.2651871740939953, 35.64915139335016647 ) ) ;
#13235 = CARTESIAN_POINT ( 'NONE',  ( 10.57123148683770175, 130.5870355106474108, -10.56118268746274325 ) ) ;
#13236 = ORIENTED_EDGE ( 'NONE', *, *, #4149, .T. ) ;
#13237 = ORIENTED_EDGE ( 'NONE', *, *, #16049, .F. ) ;
#13238 = AXIS2_PLACEMENT_3D ( 'NONE', #19483, #15845, #11211 ) ;
#13239 = CARTESIAN_POINT ( 'NONE',  ( -151.4692556286852891, -136.9891397928655010, -44.65701158161626694 ) ) ;
#13240 = ORIENTED_EDGE ( 'NONE', *, *, #18752, .F. ) ;
#13241 = CARTESIAN_POINT ( 'NONE',  ( 39.92123440845004723, 107.3344580088725877, 29.95742577749337343 ) ) ;
#13242 = CARTESIAN_POINT ( 'NONE',  ( -133.8097529055290522, 761.2091818577910090, -19.99999999999996092 ) ) ;
#13243 = VECTOR ( 'NONE', #1139, 1000.000000000000000 ) ;
#13244 = CARTESIAN_POINT ( 'NONE',  ( 39.42975644700377558, 66.07977050742731251, 31.60846029578754468 ) ) ;
#13246 = CARTESIAN_POINT ( 'NONE',  ( 21.71662816054514167, 101.4213758857254675, 8.370706496969875232 ) ) ;
#13245 = CARTESIAN_POINT ( 'NONE',  ( 46.59305225739526435, 121.3151871740940067, 36.81289934271958941 ) ) ;
#13247 = AXIS2_PLACEMENT_3D ( 'NONE', #21631, #2879, #7752 ) ;
#13248 = CARTESIAN_POINT ( 'NONE',  ( 41.46631938032478359, 82.31049967264873146, 38.96596240072933170 ) ) ;
#13249 = CARTESIAN_POINT ( 'NONE',  ( 134.6380592378699532, 268.5785371414991687, -3.999999999999996447 ) ) ;
#13250 = DIRECTION ( 'NONE',  ( 0.000000000000000000, 0.000000000000000000, 1.000000000000000000 ) ) ;
#13251 = CARTESIAN_POINT ( 'NONE',  ( 44.37947211624943833, 85.01518717409399528, 38.42115945441014446 ) ) ;
#13252 = PRODUCT_DEFINITION_CONTEXT ( 'detailed design', #11543, 'design' ) ;
#13253 = CARTESIAN_POINT ( 'NONE',  ( 129.2454342010813662, 193.1635054290503319, -44.99999999999997158 ) ) ;
#13254 = DIRECTION ( 'NONE',  ( 0.000000000000000000, 0.000000000000000000, 1.000000000000000000 ) ) ;
#13255 = ORIENTED_EDGE ( 'NONE', *, *, #13552, .F. ) ;
#13256 = CARTESIAN_POINT ( 'NONE',  ( 46.59305225739526435, 62.17977050742732104, 31.60846029578754468 ) ) ;
#13257 = CARTESIAN_POINT ( 'NONE',  ( -151.4692556286852891, -155.6438272943107393, 39.74470866294723947 ) ) ;
#13258 = VECTOR ( 'NONE', #19295, 1000.000000000000000 ) ;
#13259 = CARTESIAN_POINT ( 'NONE',  ( 20.22230697948889500, 94.36241449208007737, 1.148710122009321211 ) ) ;
#13260 = CARTESIAN_POINT ( 'NONE',  ( -160.8964159109769696, -188.3084106276440366, 46.59394152635518793 ) ) ;
#13261 = VERTEX_POINT ( 'NONE', #11174 ) ;
#13262 = CARTESIAN_POINT ( 'NONE',  ( 39.42975644700377558, 150.4151871740940010, 36.81289934271958941 ) ) ;
#13263 = EDGE_CURVE ( 'NONE', #2272, #21208, #17884, .T. ) ;
#13264 = PRESENTATION_LAYER_ASSIGNMENT (  '', '', ( #2350 ) ) ;
#13265 = LINE ( 'NONE', #15018, #7471 ) ;
#13266 = ADVANCED_FACE ( 'NONE', ( #10079 ), #8644, .F. ) ;
#13267 = CARTESIAN_POINT ( 'NONE',  ( 41.64333658814960870, 116.7797705074273296, 30.00020018409699318 ) ) ;
#13268 = CARTESIAN_POINT ( 'NONE',  ( 75.85495621331871519, 129.5603373922052697, -8.732165470513974626 ) ) ;
#13269 = VERTEX_POINT ( 'NONE', #15252 ) ;
#13270 = CARTESIAN_POINT ( 'NONE',  ( 35.25059181783574758, 92.79662968204097240, -6.272318425388238694 ) ) ;
#13271 = EDGE_LOOP ( 'NONE', ( #6962, #11610, #8365, #14546 ) ) ;
#13272 = CARTESIAN_POINT ( 'NONE',  ( 44.37947211624943833, 116.4797705074273324, 30.00020018409699318 ) ) ;
#13273 = CARTESIAN_POINT ( 'NONE',  ( 41.46631938032478359, 72.11049967264874283, 29.45539723777780239 ) ) ;
#13274 = CARTESIAN_POINT ( 'NONE',  ( 38.58424406990786082, 87.37977050742732388, 34.21067981925357060 ) ) ;
#13275 = CARTESIAN_POINT ( 'NONE',  ( 46.59305225739526435, 154.3151871740940067, 36.81289934271958941 ) ) ;
#13276 = VECTOR ( 'NONE', #3656, 1000.000000000000000 ) ;
#13277 = CARTESIAN_POINT ( 'NONE',  ( 9.248697603757472407, 114.7582530722838356, 9.914954709382596931 ) ) ;
#13278 = CARTESIAN_POINT ( 'NONE',  ( -141.4692556286852891, -195.0630981290893260, 49.65701158161630957 ) ) ;
#13279 = DIRECTION ( 'NONE',  ( 0.000000000000000000, 0.000000000000000000, -1.000000000000000000 ) ) ;
#13280 = FACE_OUTER_BOUND ( 'NONE', #21297, .T. ) ;
#13281 = CARTESIAN_POINT ( 'NONE',  ( -148.3790856849358306, -177.3891397928654783, 40.14644641866477315 ) ) ;
#13282 = CARTESIAN_POINT ( 'NONE',  ( 39.92123440845005433, 156.2604996726487059, 29.95742577749336988 ) ) ;
#13283 = CARTESIAN_POINT ( 'NONE',  ( 41.46631938032478359, 102.1104996726487286, 29.45539723777780239 ) ) ;
#13284 = CARTESIAN_POINT ( 'NONE',  ( -145.6429501568359797, -194.9438272943107222, 41.63779006702063867 ) ) ;
#13285 = CONTEXT_DEPENDENT_SHAPE_REPRESENTATION ( #697, #2892 ) ;
#13286 = CARTESIAN_POINT ( 'NONE',  ( 41.64333658814960870, 95.77977050742732956, 30.00020018409699318 ) ) ;
#13287 = CARTESIAN_POINT ( 'NONE',  ( 53.47116958538193643, 146.1823035489369715, 17.34243072007611985 ) ) ;
#13288 = CARTESIAN_POINT ( 'NONE',  ( -151.4692556286852891, -187.1438272943106824, 59.56931450028537967 ) ) ;
#13289 = CIRCLE ( 'NONE', #11880, 27.58651506682278765 ) ;
#13290 = EDGE_LOOP ( 'NONE', ( #8205, #20115, #19435, #16756 ) ) ;
#13291 = CARTESIAN_POINT ( 'NONE',  ( 38.01140435219952707, 137.9344580088725820, 35.83527830041809636 ) ) ;
#13292 = CARTESIAN_POINT ( 'NONE',  ( 8.829984022807513711, 121.7968051057545580, 16.14860047415989541 ) ) ;
#13293 = CARTESIAN_POINT ( 'NONE',  ( 46.59305225739526435, 140.1797705074273210, 31.60846029578754468 ) ) ;
#13294 = CARTESIAN_POINT ( 'NONE',  ( 69.89089498905519804, 111.6491328518190613, -0.005813817042542732995 ) ) ;
#13295 = CIRCLE ( 'NONE', #16094, 24.99999999999999289 ) ;
#13296 = PRODUCT ( 'Cast Steel Heavy Body Block', 'Cast Steel Heavy Body Block', '', ( #14920 ) ) ;
#13297 = CARTESIAN_POINT ( 'NONE',  ( 38.58424406990785371, 66.22977050742730398, 32.77220824515697473 ) ) ;
#13298 = EDGE_LOOP ( 'NONE', ( #13792, #15391, #10638, #4947 ) ) ;
#13299 = CARTESIAN_POINT ( 'NONE',  ( 38.58424406990784661, 144.2297705074273324, 32.77220824515698183 ) ) ;
#13300 = CARTESIAN_POINT ( 'NONE',  ( -151.4692556286852607, -171.2391397928654726, 39.65701158161629536 ) ) ;
#13301 = VECTOR ( 'NONE', #21677, 1000.000000000000000 ) ;
#13302 = CARTESIAN_POINT ( 'NONE',  ( 41.46631938032478359, 115.3104996726487599, 38.96596240072933170 ) ) ;
#13303 = CARTESIAN_POINT ( 'NONE',  ( 46.59305225739526435, 70.31518717409400665, 36.81289934271958941 ) ) ;
#13304 = CARTESIAN_POINT ( 'NONE',  ( 38.01140435219952707, 95.93445800887258201, 35.83527830041809636 ) ) ;
#13305 = CARTESIAN_POINT ( 'NONE',  ( -151.4692556286852891, -157.1438272943107393, 59.56931450028537256 ) ) ;
#13306 = CIRCLE ( 'NONE', #7688, 10.00000000000000888 ) ;
#13307 = CARTESIAN_POINT ( 'NONE',  ( -143.3790856849358306, -165.6891397928654897, 43.77915905869157598 ) ) ;
#13308 = CARTESIAN_POINT ( 'NONE',  ( -148.3790856849358306, -179.4630981290893033, 40.14644641866477315 ) ) ;
#13309 = EDGE_CURVE ( 'NONE', #4102, #16674, #2623, .T. ) ;
#13310 = CARTESIAN_POINT ( 'NONE',  ( -161.4692556286852891, -191.6391397928654499, 46.40781461928724383 ) ) ;
#13311 = CARTESIAN_POINT ( 'NONE',  ( 48.01140435219951996, 154.4344580088725820, 32.58608133808903773 ) ) ;
#13312 = CARTESIAN_POINT ( 'NONE',  ( 45.74753988029933538, 122.3297705074273267, 30.44471234641811819 ) ) ;
#13313 = CARTESIAN_POINT ( 'NONE',  ( 59.95958160670890180, 90.07020311440788873, 19.76341270931769500 ) ) ;
#13314 = CARTESIAN_POINT ( 'NONE',  ( 38.58424406990785371, 117.2651871740940095, 35.64915139335015937 ) ) ;
#13315 = DIRECTION ( 'NONE',  ( 1.000000000000000000, 0.000000000000000000, 0.000000000000000000 ) ) ;
#13316 = DIRECTION ( 'NONE',  ( -0.000000000000000000, -0.000000000000000000, 1.000000000000000000 ) ) ;
#13317 = CARTESIAN_POINT ( 'NONE',  ( 62.47932545177000208, 147.9683691103492436, 5.510132816154444946 ) ) ;
#13318 = CARTESIAN_POINT ( 'NONE',  ( 52.49585387951581339, 146.4637788833130685, -2.700609006624497876 ) ) ;
#13319 = CARTESIAN_POINT ( 'NONE',  ( -151.4692556286852891, -185.3130981290893260, 39.65701158161630246 ) ) ;
#13320 = CARTESIAN_POINT ( 'NONE',  ( 47.43856463449117911, 95.02977050742730114, 32.77220824515697473 ) ) ;
#13321 = ORIENTED_EDGE ( 'NONE', *, *, #13500, .T. ) ;
#13322 = PRESENTATION_LAYER_ASSIGNMENT (  '', '', ( #20026 ) ) ;
#13323 = CARTESIAN_POINT ( 'NONE',  ( 46.10157429594899270, 145.7344580088725650, 29.95742577749336988 ) ) ;
#13324 = ORIENTED_EDGE ( 'NONE', *, *, #588, .F. ) ;
#13325 =( BOUNDED_CURVE ( )  B_SPLINE_CURVE ( 2, ( #17625, #15969, #880, #1427, #20069, #4956, #6732, #3301, #14860, #8155, #8268, #16510, #4615 ),
 .UNSPECIFIED., .F., .F. ) 
 B_SPLINE_CURVE_WITH_KNOTS ( ( 3, 2, 2, 2, 2, 2, 3 ),
 ( 0.6607142857142856984, 0.6642857142857142572, 0.6714285714285713746, 0.6785714285714286031, 0.6857142857142857206, 0.6928571428571428381, 0.6964285714285713969 ),
 .UNSPECIFIED. ) 
 CURVE ( )  GEOMETRIC_REPRESENTATION_ITEM ( )  RATIONAL_B_SPLINE_CURVE ( ( 0.9755282581475768211, 0.9755282581475768211, 1.000000000000000000, 0.9510565162951535312, 1.000000000000000000, 0.9510565162951535312, 1.000000000000000000, 0.9510565162951535312, 1.000000000000000000, 0.9510565162951535312, 1.000000000000000000, 0.9755282581475768211, 0.9755282581475768211 ) ) 
 REPRESENTATION_ITEM ( '' )  );
#13326 = CARTESIAN_POINT ( 'NONE',  ( 38.01140435219951996, 80.63445800887258486, 32.58608133808903773 ) ) ;
#13327 = CARTESIAN_POINT ( 'NONE',  ( 38.96631938032478359, 60.08445800887257349, 37.14960608071593384 ) ) ;
#13328 = CARTESIAN_POINT ( 'NONE',  ( 39.92123440845004723, 141.2604996726487627, 29.95742577749337343 ) ) ;
#13330 = CARTESIAN_POINT ( 'NONE',  ( 67.19681472375953035, 134.2522627023263908, 6.065787011912938453 ) ) ;
#13329 = CARTESIAN_POINT ( 'NONE',  ( 39.42975644700377558, 96.41518717409400097, 36.81289934271958941 ) ) ;
#13331 = CARTESIAN_POINT ( 'NONE',  ( -160.8964159109769696, -170.0084106276440252, 52.72008163687743121 ) ) ;
#13332 = CARTESIAN_POINT ( 'NONE',  ( -143.8425227516148084, -186.0938272943107279, 44.11586579668791330 ) ) ;
#13334 = CYLINDRICAL_SURFACE ( 'NONE', #8672, 10.00000000000000888 ) ;
#13333 = CARTESIAN_POINT ( 'NONE',  ( 43.01140435219951996, 155.9604996726487514, 29.21067981925357060 ) ) ;
#13335 = CARTESIAN_POINT ( 'NONE',  ( 42.21948215057684450, 147.0373810949689926, 29.21067981925356705 ) ) ;
#13336 = CARTESIAN_POINT ( 'NONE',  ( 48.01140435219951996, 80.06049967264871725, 35.83527830041809636 ) ) ;
#13337 = CARTESIAN_POINT ( 'NONE',  ( 44.37947211624943833, 62.21518717409399102, 30.00020018409699318 ) ) ;
#13338 = DIRECTION ( 'NONE',  ( 0.000000000000000000, 0.000000000000000000, 1.000000000000000000 ) ) ;
#13339 = CARTESIAN_POINT ( 'NONE',  ( 40.02721236285810136, 85.80382532021769748, 0.4343372985580923329 ) ) ;
#13340 = CARTESIAN_POINT ( 'NONE',  ( 39.42975644700377558, 147.4151871740940294, 36.81289934271958941 ) ) ;
#13341 = CARTESIAN_POINT ( 'NONE',  ( -151.4692556286852891, -161.6438272943107393, 39.74470866294723947 ) ) ;
#13342 = CARTESIAN_POINT ( 'NONE',  ( -145.6429501568359797, -178.1084106276440480, 57.67623309621197336 ) ) ;
#13343 = ORIENTED_EDGE ( 'NONE', *, *, #16951, .T. ) ;
#13344 = CARTESIAN_POINT ( 'NONE',  ( 41.46631938032478359, 78.38445800887257064, 38.96596240072933170 ) ) ;
#13345 = CARTESIAN_POINT ( 'NONE',  ( -160.8964159109769696, -164.3084106276440650, 46.59394152635518793 ) ) ;
#13346 = CARTESIAN_POINT ( 'NONE',  ( 16.32863300717066579, 110.5331391746388761, 0.7949662885976053195 ) ) ;
#13347 = CYLINDRICAL_SURFACE ( 'NONE', #6345, 4.999999999999997335 ) ;
#13348 = CARTESIAN_POINT ( 'NONE',  ( 47.43856463449117200, 124.7651871740939811, 32.77220824515698183 ) ) ;
#13349 = CARTESIAN_POINT ( 'NONE',  ( 20.63953418349755253, 94.10117616956034681, -11.87063135391590052 ) ) ;
#13350 = ORIENTED_EDGE ( 'NONE', *, *, #1837, .T. ) ;
#13351 = VERTEX_POINT ( 'NONE', #3677 ) ;
#13352 = CARTESIAN_POINT ( 'NONE',  ( -148.3790856849358306, -192.3891397928654783, 40.14644641866477315 ) ) ;
#13353 = VERTEX_POINT ( 'NONE', #17107 ) ;
#13354 = CIRCLE ( 'NONE', #1745, 5.000000000000004441 ) ;
#13355 = CARTESIAN_POINT ( 'NONE',  ( 40.27526882409969033, 63.82977050742731961, 37.97664729208901946 ) ) ;
#13357 = CARTESIAN_POINT ( 'NONE',  ( 54.67410106651116308, 94.23276814491528341, 6.942135068398441078 ) ) ;
#13356 = CARTESIAN_POINT ( 'NONE',  ( 47.43856463449117200, 124.7651871740939811, 32.77220824515698183 ) ) ;
#13358 = CARTESIAN_POINT ( 'NONE',  ( 44.55648932407425633, 79.61049967264874283, 38.96596240072933170 ) ) ;
#13359 = FACE_OUTER_BOUND ( 'NONE', #6064, .T. ) ;
#13360 = CYLINDRICAL_SURFACE ( 'NONE', #2603, 4.999999999999997335 ) ;
#13361 = DIRECTION ( 'NONE',  ( -0.000000000000000000, 1.000000000000000000, -0.000000000000000000 ) ) ;
#13362 = CARTESIAN_POINT ( 'NONE',  ( 40.27526882409969033, 87.56518717409400665, 37.97664729208901946 ) ) ;
#13363 = CARTESIAN_POINT ( 'NONE',  ( 157.5268905834513475, 193.0332408774651185, -49.99999999999997158 ) ) ;
#13364 = DIRECTION ( 'NONE',  ( 0.4938165983075534227, -0.8695660798558993987, 0.000000000000000000 ) ) ;
#13365 = EDGE_CURVE ( 'NONE', #13351, #14655, #2334, .T. ) ;
#13366 = ORIENTED_EDGE ( 'NONE', *, *, #21507, .F. ) ;
#13367 = CARTESIAN_POINT ( 'NONE',  ( 47.43856463449117200, 67.72977050742731819, 35.64915139335016647 ) ) ;
#13368 = CARTESIAN_POINT ( 'NONE',  ( -143.8425227516148084, -189.3584106276440480, 44.11586579668791330 ) ) ;
#13369 = CARTESIAN_POINT ( 'NONE',  ( 8.869018199820361659, 117.4101421016551967, 9.005765870029716069 ) ) ;
#13370 = CARTESIAN_POINT ( 'NONE',  ( -148.5561028927606344, -177.0584106276440366, 40.69124936498395328 ) ) ;
#13371 = EDGE_LOOP ( 'NONE', ( #982, #12966, #21570, #6517 ) ) ;
#13372 = CARTESIAN_POINT ( 'NONE',  ( 46.59305225739526435, 154.9151871740940010, 31.60846029578754468 ) ) ;
#13373 = CARTESIAN_POINT ( 'NONE',  ( -145.2889157411863437, -160.4391397928654612, 58.16351966513671812 ) ) ;
#13374 = CARTESIAN_POINT ( 'NONE',  ( 43.01140435219951286, 112.1297705074272812, 38.86567161673127657 ) ) ;
#13375 = CARTESIAN_POINT ( 'NONE',  ( 47.05648932407426344, 154.5844580088725877, 31.27175355779120025 ) ) ;
#13376 = VERTEX_POINT ( 'NONE', #15139 ) ;
#13377 = CARTESIAN_POINT ( 'NONE',  ( 31.34884810169724645, 145.5825485123889109, -10.55804779818428862 ) ) ;
#13378 = VERTEX_POINT ( 'NONE', #1809 ) ;
#13379 = CARTESIAN_POINT ( 'NONE',  ( 38.01140435219952707, 126.8604996726487002, 35.83527830041809636 ) ) ;
#13380 = ADVANCED_FACE ( 'NONE', ( #17000 ), #6883, .T. ) ;
#13381 = CARTESIAN_POINT ( 'NONE',  ( 38.58424406990784661, 150.2651871740940237, 35.64915139335016647 ) ) ;
#13382 = CARTESIAN_POINT ( 'NONE',  ( 71.14040157825178312, 139.4183699182763974, -9.089337262093875935 ) ) ;
#13383 = CLOSED_SHELL ( 'NONE', ( #13551, #16106, #5631, #20806, #19190, #8936, #9175, #7500, #2284, #14826, #1115, #18913, #2105, #6871, #1061, #4837, #5099, #9999, #7228, #6963, #7645, #18414, #5033, #1739 ) ) ;
#13384 = PRODUCT_DEFINITION_FORMATION_WITH_SPECIFIED_SOURCE ( 'ANY', '', #21567, .NOT_KNOWN. ) ;
#13385 = LINE ( 'NONE', #15447, #15392 ) ;
#13386 = DIRECTION ( 'NONE',  ( -0.000000000000000000, 1.000000000000000000, -0.000000000000000000 ) ) ;
#13387 = CARTESIAN_POINT ( 'NONE',  ( -130.4480969619998234, -126.9891397928655010, 67.64809332337415526 ) ) ;
#13388 = CARTESIAN_POINT ( 'NONE',  ( -154.5594255724347761, -178.8891397928654783, 59.16757674456785310 ) ) ;
#13389 = EDGE_CURVE ( 'NONE', #11299, #7475, #14149, .T. ) ;
#13390 = CARTESIAN_POINT ( 'NONE',  ( 43.01140435219951286, 89.03445800887257633, 29.21067981925356705 ) ) ;
#13391 = DIRECTION ( 'NONE',  ( -0.000000000000000000, 1.000000000000000000, -0.000000000000000000 ) ) ;
#13392 = CARTESIAN_POINT ( 'NONE',  ( 43.80332655382220253, 97.95757658655229250, 29.21067981925356705 ) ) ;
#13393 = CARTESIAN_POINT ( 'NONE',  ( 47.43856463449117200, 92.02977050742730114, 32.77220824515698183 ) ) ;
#13394 = CARTESIAN_POINT ( 'NONE',  ( 19.58029209685692962, 104.0714924419353480, 21.50917333468608561 ) ) ;
#13395 = CARTESIAN_POINT ( 'NONE',  ( -151.4692556286852891, -176.6438272943107393, 39.74470866294723947 ) ) ;
#13396 = CARTESIAN_POINT ( 'NONE',  ( 47.43856463449117911, 88.76518717409399528, 32.77220824515697473 ) ) ;
#13397 = DIRECTION ( 'NONE',  ( 1.000000000000000000, 0.000000000000000000, 0.000000000000000000 ) ) ;
#13398 = VERTEX_POINT ( 'NONE', #20328 ) ;
#13399 = DIRECTION ( 'NONE',  ( -0.000000000000000000, -0.000000000000000000, -1.000000000000000000 ) ) ;
#13400 = CARTESIAN_POINT ( 'NONE',  ( 14.88286428391304561, 100.3963227437532595, 8.410691821786379307 ) ) ;
#13401 = CARTESIAN_POINT ( 'NONE',  ( 44.37947211624943833, 139.2797705074273154, 38.42115945441014446 ) ) ;
#13402 = CARTESIAN_POINT ( 'NONE',  ( 14.95244176413730131, 118.0514569880088231, 3.089472225200239563 ) ) ;
#13403 = CLOSED_SHELL ( 'NONE', ( #4668, #16986, #9320, #10830, #2995, #3355, #1069, #5684, #14740, #20166 ) ) ;
#13404 = CARTESIAN_POINT ( 'NONE',  ( -145.6429501568359797, -191.9438272943106938, 41.63779006702063867 ) ) ;
#13405 = CARTESIAN_POINT ( 'NONE',  ( 45.22505347682923116, 59.38050100342834270, 30.37668637662395099 ) ) ;
#13406 = VERTEX_POINT ( 'NONE', #371 ) ;
#13407 = CARTESIAN_POINT ( 'NONE',  ( 40.27526882409969033, 149.9297705074272926, 30.44471234641811819 ) ) ;
#13408 = CARTESIAN_POINT ( 'NONE',  ( 83.67254549292280785, -61.68114226949890622, -46.21320343559645494 ) ) ;
#13409 = EDGE_CURVE ( 'NONE', #11879, #12307, #18562, .T. ) ;
#13410 = CARTESIAN_POINT ( 'NONE',  ( 38.96631938032478359, 108.4104996726487400, 31.27175355779120025 ) ) ;
#13411 = CARTESIAN_POINT ( 'NONE',  ( 180.1254907973641934, 54.87273858953557237, 4.000000000000021316 ) ) ;
#13412 = CARTESIAN_POINT ( 'NONE',  ( -143.7724355939531904, 531.4176628826018032, -19.99999999999997868 ) ) ;
#13413 = CARTESIAN_POINT ( 'NONE',  ( -142.0420953463935803, -165.2438272943107052, 46.59394152635518083 ) ) ;
#13414 = CARTESIAN_POINT ( 'NONE',  ( 38.01140435219952707, 122.6344580088725849, 32.58608133808903773 ) ) ;
#13415 = CARTESIAN_POINT ( 'NONE',  ( -141.4692556286852891, -167.9130981290892635, 46.40781461928724383 ) ) ;
#13416 = CARTESIAN_POINT ( 'NONE',  ( 46.10157429594899270, 154.7344580088725650, 29.95742577749337343 ) ) ;
#13417 = CARTESIAN_POINT ( 'NONE',  ( 46.59305225739526435, 118.5797705074273267, 36.81289934271958941 ) ) ;
#13418 = CARTESIAN_POINT ( 'NONE',  ( 17.22388115030108224, 97.27017246186569821, 14.28717435998666296 ) ) ;
#13419 = DIRECTION ( 'NONE',  ( -0.9385982292947089300, -0.3450121214752274734, 0.000000000000000000 ) ) ;
#13420 = CARTESIAN_POINT ( 'NONE',  ( 44.37947211624943833, 112.0151871740940095, 38.42115945441014446 ) ) ;
#13421 = CARTESIAN_POINT ( 'NONE',  ( -157.6495955161842062, -167.9391397928654897, 41.15050349809589392 ) ) ;
#13422 = CARTESIAN_POINT ( 'NONE',  ( 43.01140435219951996, 10.71049967264875491, 29.21067981925357060 ) ) ;
#13423 = CARTESIAN_POINT ( 'NONE',  ( 51.97100187899584967, 152.8641821122263309, -1.870631353872792335 ) ) ;
#13424 = CARTESIAN_POINT ( 'NONE',  ( 29.12819380265916180, 95.36133955912156068, 0.9897074016940036190 ) ) ;
#13425 = CARTESIAN_POINT ( 'NONE',  ( -149.8854112254399240, -155.3899795514095672, 39.65701158161629536 ) ) ;
#13426 = CARTESIAN_POINT ( 'NONE',  ( 38.58424406990785371, 84.22977050742730398, 32.77220824515697473 ) ) ;
#13427 = EDGE_LOOP ( 'NONE', ( #10696, #1357, #169, #21754, #18636, #16661, #19801, #19490 ) ) ;
#13428 = EDGE_CURVE ( 'NONE', #7232, #17291, #2675, .T. ) ;
#13429 = CARTESIAN_POINT ( 'NONE',  ( 0.000000000000000000, 0.000000000000000000, 30.00000000000000000 ) ) ;
#13430 = VERTEX_POINT ( 'NONE', #11718 ) ;
#13431 = CARTESIAN_POINT ( 'NONE',  ( 48.01140435219951996, 76.28445800887257633, 34.21067981925357060 ) ) ;
#13432 = DIRECTION ( 'NONE',  ( 1.000000000000000000, 0.000000000000000000, 0.000000000000000000 ) ) ;
#13433 = CARTESIAN_POINT ( 'NONE',  ( 48.01140435219951996, 137.3604996726487570, 32.58608133808903773 ) ) ;
#13435 = CARTESIAN_POINT ( 'NONE',  ( 23.40005864183818218, 147.8691531402271835, -9.846981161663094895 ) ) ;
#13434 = CARTESIAN_POINT ( 'NONE',  ( 46.59305225739526435, 97.31518717409400665, 36.81289934271958941 ) ) ;
#13436 = CARTESIAN_POINT ( 'NONE',  ( -154.3824083646099439, -167.7584106276440536, 40.69124936498395328 ) ) ;
#13437 = CARTESIAN_POINT ( 'NONE',  ( -143.8425227516148084, -189.0938272943107279, 44.11586579668791330 ) ) ;
#13438 = CARTESIAN_POINT ( 'NONE',  ( 43.01140435219951286, 69.53445800887257633, 39.21067981925356349 ) ) ;
#13439 = DIRECTION ( 'NONE',  ( -1.000000000000000000, 0.000000000000000000, -5.966140889015784385E-16 ) ) ;
#13440 = VECTOR ( 'NONE', #16437, 1000.000000000000000 ) ;
#13441 = VECTOR ( 'NONE', #17449, 1000.000000000000000 ) ;
#13442 = CARTESIAN_POINT ( 'NONE',  ( -151.4692556286852891, -126.9891397928655010, 49.65701158161630957 ) ) ;
#13443 = CARTESIAN_POINT ( 'NONE',  ( 43.80332655382220253, 79.53738109496900677, 39.21067981925355639 ) ) ;
#13444 = CARTESIAN_POINT ( 'NONE',  ( 41.64333658814960870, 153.9797705074273324, 38.42115945441014446 ) ) ;
#13445 = CARTESIAN_POINT ( 'NONE',  ( 38.96631938032478359, 62.48445800887257917, 31.27175355779120025 ) ) ;
#13446 = CARTESIAN_POINT ( 'NONE',  ( 17.60877916486148465, 96.95950790538488206, 1.267834678905774393 ) ) ;
#13447 = CARTESIAN_POINT ( 'NONE',  ( 46.59305225739526435, 148.3151871740940067, 36.81289934271958941 ) ) ;
#13448 = VECTOR ( 'NONE', #11414, 1000.000000000000000 ) ;
#13449 = CARTESIAN_POINT ( 'NONE',  ( -142.0420953463935803, -159.2438272943107620, 46.59394152635518793 ) ) ;
#13450 = CARTESIAN_POINT ( 'NONE',  ( -157.2955611005345986, -175.7084106276440707, 57.67623309621197336 ) ) ;
#13451 = ORIENTED_EDGE ( 'NONE', *, *, #1011, .F. ) ;
#13452 = CARTESIAN_POINT ( 'NONE',  ( 44.37947211624943833, 62.21518717409399102, 30.00020018409699318 ) ) ;
#13453 = CARTESIAN_POINT ( 'NONE',  ( -157.2955611005346270, -163.7084106276440139, 57.67623309621198047 ) ) ;
#13454 = CARTESIAN_POINT ( 'NONE',  ( 24.57236314005146838, 141.2733614120550385, -4.872173989822636386 ) ) ;
#13455 = CARTESIAN_POINT ( 'NONE',  ( 41.64333658814960870, 123.7151871740940123, 38.42115945441014446 ) ) ;
#13456 =( BOUNDED_CURVE ( )  B_SPLINE_CURVE ( 2, ( #9053, #18647, #20303, #17192, #453, #11918, #3549, #10275, #16977, #1887, #4083, #12890, #16188 ),
 .UNSPECIFIED., .F., .F. ) 
 B_SPLINE_CURVE_WITH_KNOTS ( ( 3, 2, 2, 2, 2, 2, 3 ),
 ( 0.09558823529411764053, 0.09705882352941176683, 0.1000000000000000056, 0.1029411764705882304, 0.1058823529411764691, 0.1088235294117647078, 0.1102941176470588203 ),
 .UNSPECIFIED. ) 
 CURVE ( )  GEOMETRIC_REPRESENTATION_ITEM ( )  RATIONAL_B_SPLINE_CURVE ( ( 0.9755282581475767101, 0.9755282581475765991, 1.000000000000000000, 0.9510565162951535312, 1.000000000000000000, 0.9510565162951535312, 1.000000000000000000, 0.9510565162951535312, 1.000000000000000000, 0.9510565162951535312, 1.000000000000000000, 0.9755282581475768211, 0.9755282581475767101 ) ) 
 REPRESENTATION_ITEM ( '' )  );
#13457 = ORIENTED_EDGE ( 'NONE', *, *, #16105, .F. ) ;
#13458 = EDGE_LOOP ( 'NONE', ( #8144, #13457, #9394, #1171 ) ) ;
#13459 = EDGE_CURVE ( 'NONE', #17105, #5159, #16895, .T. ) ;
#13460 = AXIS2_PLACEMENT_3D ( 'NONE', #13764, #17178, #3749 ) ;
#13461 = CARTESIAN_POINT ( 'NONE',  ( -145.2889157411863437, -193.4391397928654612, 58.16351966513671812 ) ) ;
#13462 = VERTEX_POINT ( 'NONE', #11941 ) ;
#13463 = CARTESIAN_POINT ( 'NONE',  ( 43.01140435219951286, 70.12977050742732388, 38.86567161673127657 ) ) ;
#13465 = CARTESIAN_POINT ( 'NONE',  ( 20.99626426110969390, 137.5292218135913913, 9.918250401459649979 ) ) ;
#13464 = CARTESIAN_POINT ( 'NONE',  ( 46.59305225739526435, 121.9151871740940010, 31.60846029578754468 ) ) ;
#13466 = EDGE_CURVE ( 'NONE', #9846, #3209, #3573, .T. ) ;
#13467 = CARTESIAN_POINT ( 'NONE',  ( 48.01140435219951996, 83.36049967264872862, 32.58608133808903773 ) ) ;
#13468 = FACE_OUTER_BOUND ( 'NONE', #16119, .T. ) ;
#13469 = CARTESIAN_POINT ( 'NONE',  ( 47.05648932407426344, 97.91049967264873999, 37.14960608071593384 ) ) ;
#13470 = DIRECTION ( 'NONE',  ( -0.000000000000000000, 1.000000000000000000, -0.000000000000000000 ) ) ;
#13471 = CARTESIAN_POINT ( 'NONE',  ( 40.27526882409969033, 77.66518717409400097, 30.44471234641811819 ) ) ;
#13472 = CARTESIAN_POINT ( 'NONE',  ( 40.50423473544901753, 144.7825417035512601, 38.54896506029345460 ) ) ;
#13473 = CARTESIAN_POINT ( 'NONE',  ( 148.6725454929228079, -61.68114226949890622, 10.00000000000001599 ) ) ;
#13474 = ORIENTED_EDGE ( 'NONE', *, *, #21595, .F. ) ;
#13475 = CARTESIAN_POINT ( 'NONE',  ( 40.27526882409969033, 66.82977050742732672, 37.97664729208901946 ) ) ;
#13476 = CARTESIAN_POINT ( 'NONE',  ( -145.6429501568359797, -183.2084106276440423, 41.63779006702063867 ) ) ;
#13477 = CARTESIAN_POINT ( 'NONE',  ( 77.31131846045057898, 118.9338434746808844, -2.379532457331845485 ) ) ;
#13478 = CARTESIAN_POINT ( 'NONE',  ( -151.4692556286852891, -176.9084106276440309, 39.74470866294723947 ) ) ;
#13479 = ADVANCED_BREP_SHAPE_REPRESENTATION ( '', ( #14549, #353, #12657 ), #19020 ) ;
#13480 = ORIENTED_EDGE ( 'NONE', *, *, #7891, .F. ) ;
#13481 = CARTESIAN_POINT ( 'NONE',  ( 44.37947211624943833, 155.2151871740940123, 30.00020018409699318 ) ) ;
#13482 = DIRECTION ( 'NONE',  ( 0.3450121214752278065, -0.9385982292947087080, 0.000000000000000000 ) ) ;
#13483 = CARTESIAN_POINT ( 'NONE',  ( 45.74753988029934249, 110.3297705074273125, 30.44471234641812174 ) ) ;
#13484 = CARTESIAN_POINT ( 'NONE',  ( 23.23160898551418185, 147.7622765488190453, -10.85157364460736140 ) ) ;
#13485 = VERTEX_POINT ( 'NONE', #15569 ) ;
#13486 = CARTESIAN_POINT ( 'NONE',  ( 52.49585387951581339, 146.4637788833130685, -2.700609006624497876 ) ) ;
#13487 = VERTEX_POINT ( 'NONE', #2445 ) ;
#13488 = CARTESIAN_POINT ( 'NONE',  ( 41.64333658814960870, 117.9797705074273182, 38.42115945441014446 ) ) ;
#13489 = DIRECTION ( 'NONE',  ( -0.000000000000000000, -0.000000000000000000, -1.000000000000000000 ) ) ;
#13490 = CARTESIAN_POINT ( 'NONE',  ( 38.58424406990784661, 87.52977050742730114, 35.64915139335016647 ) ) ;
#13491 = CARTESIAN_POINT ( 'NONE',  ( 39.42975644700377558, 156.4151871740940010, 36.81289934271958941 ) ) ;
#13492 = EDGE_CURVE ( 'NONE', #14908, #4098, #7285, .T. ) ;
#13493 = CARTESIAN_POINT ( 'NONE',  ( 65.38231449488820601, 145.7134111962467671, 5.629255361809699210 ) ) ;
#13494 = DIRECTION ( 'NONE',  ( -0.3450121214752278620, 0.9385982292947087080, 0.000000000000000000 ) ) ;
#13495 = CARTESIAN_POINT ( 'NONE',  ( -141.4692556286852891, -175.1391397928654783, 52.90620854394536821 ) ) ;
#13496 = CARTESIAN_POINT ( 'NONE',  ( -157.6495955161842062, -181.1130981290893089, 58.16351966513671812 ) ) ;
#13497 = UNCERTAINTY_MEASURE_WITH_UNIT (LENGTH_MEASURE( 1.000000000000000082E-05 ), #857, 'distance_accuracy_value', 'NONE');
#13498 = FACE_OUTER_BOUND ( 'NONE', #13788, .T. ) ;
#13499 = CARTESIAN_POINT ( 'NONE',  ( 48.01140435219951996, 77.36049967264874283, 32.58608133808903773 ) ) ;
#13500 = EDGE_CURVE ( 'NONE', #5138, #21295, #11843, .T. ) ;
#13501 = CARTESIAN_POINT ( 'NONE',  ( 39.42975644700377558, 90.07977050742732672, 31.60846029578754468 ) ) ;
#13502 = CARTESIAN_POINT ( 'NONE',  ( 15.50679444821833819, 113.6848169819070193, -5.081469017220888063 ) ) ;
#13503 = CARTESIAN_POINT ( 'NONE',  ( -160.8964159109769696, -169.8938272943107393, 49.65701158161630957 ) ) ;
#13504 = CARTESIAN_POINT ( 'NONE',  ( 39.42975644700377558, 86.81518717409400665, 31.60846029578754468 ) ) ;
#13505 = LINE ( 'NONE', #1715, #9372 ) ;
#13506 = EDGE_LOOP ( 'NONE', ( #13144, #6427, #2256, #223 ) ) ;
#13507 = CARTESIAN_POINT ( 'NONE',  ( 38.01140435219952707, 137.7844580088726048, 34.21067981925357060 ) ) ;
#13508 = CARTESIAN_POINT ( 'NONE',  ( 22.46358530849972723, 92.52609567587644790, 8.053519324161520387 ) ) ;
#13509 = EDGE_CURVE ( 'NONE', #13722, #12813, #11489, .T. ) ;
#13510 = CARTESIAN_POINT ( 'NONE',  ( 41.64333658814960870, 138.9797705074273324, 38.42115945441014446 ) ) ;
#13511 = CARTESIAN_POINT ( 'NONE',  ( 16.71508173162657229, 129.8698440624217483, 3.565528294796503683 ) ) ;
#13512 = CARTESIAN_POINT ( 'NONE',  ( 148.6725454929228079, -61.68114226949890622, -16.21320343559643717 ) ) ;
#13513 = VERTEX_POINT ( 'NONE', #17325 ) ;
#13514 = CARTESIAN_POINT ( 'NONE',  ( 38.58424406990784661, 150.2297705074273040, 32.77220824515698183 ) ) ;
#13515 = CARTESIAN_POINT ( 'NONE',  ( 41.64333658814960870, 93.97977050742733240, 38.42115945441014446 ) ) ;
#13516 = CARTESIAN_POINT ( 'NONE',  ( 46.10157429594899270, 152.6604996726487400, 29.95742577749336988 ) ) ;
#13517 = DIRECTION ( 'NONE',  ( 1.000000000000000000, 0.000000000000000000, 0.000000000000000000 ) ) ;
#13518 = CARTESIAN_POINT ( 'NONE',  ( -161.4692556286853176, -169.5630981290893260, 49.65701158161630957 ) ) ;
#13519 = CARTESIAN_POINT ( 'NONE',  ( -143.3790856849358306, -173.7630981290892862, 43.77915905869157598 ) ) ;
#13520 = DIRECTION ( 'NONE',  ( 0.000000000000000000, -1.000000000000000000, 0.000000000000000000 ) ) ;
#13521 = CARTESIAN_POINT ( 'NONE',  ( -161.4692556286852607, -166.4130981290893203, 52.90620854394536821 ) ) ;
#13522 = CARTESIAN_POINT ( 'NONE',  ( 39.92123440845004723, 141.2344580088725365, 38.46393386101376421 ) ) ;
#13523 = CARTESIAN_POINT ( 'NONE',  ( 45.74753988029933538, 121.4297705074273068, 37.97664729208901946 ) ) ;
#13524 = CARTESIAN_POINT ( 'NONE',  ( 38.74908582987571748, 85.85911260889788821, 20.47761041045779606 ) ) ;
#13525 = CARTESIAN_POINT ( 'NONE',  ( -143.3790856849358306, -183.6891397928654612, 43.77915905869157598 ) ) ;
#13526 = CARTESIAN_POINT ( 'NONE',  ( 41.64333658814960870, 119.5151871740940095, 30.00020018409699318 ) ) ;
#13527 = DIRECTION ( 'NONE',  ( 1.000000000000000000, 0.000000000000000000, 0.000000000000000000 ) ) ;
#13528 = CARTESIAN_POINT ( 'NONE',  ( 77.16427934405430733, 119.9933672671919851, 6.581674455321548933 ) ) ;
#13529 = CARTESIAN_POINT ( 'NONE',  ( 16.16443657470430750, 128.5343009702184816, -4.486436360144259616 ) ) ;
#13530 = CARTESIAN_POINT ( 'NONE',  ( -145.2889157411863437, -186.5130981290893146, 58.16351966513671812 ) ) ;
#13531 = CARTESIAN_POINT ( 'NONE',  ( 44.37947211624943833, 82.27977050742732956, 38.42115945441014446 ) ) ;
#13532 = EDGE_CURVE ( 'NONE', #7289, #5516, #17535, .T. ) ;
#13533 = VERTEX_POINT ( 'NONE', #12260 ) ;
#13534 = DIRECTION ( 'NONE',  ( 0.000000000000000000, -1.000000000000000000, 0.000000000000000000 ) ) ;
#13535 = CARTESIAN_POINT ( 'NONE',  ( 38.96631938032478359, 74.48445800887257917, 31.27175355779120025 ) ) ;
#13536 = CARTESIAN_POINT ( 'NONE',  ( 39.92123440845005433, 87.23445800887257917, 38.46393386101375711 ) ) ;
#13537 = CARTESIAN_POINT ( 'NONE',  ( 44.55648932407425633, 134.8104996726487457, 29.45539723777780239 ) ) ;
#13539 = CARTESIAN_POINT ( 'NONE',  ( 75.83902229129397199, 129.3300604911257778, -14.72777435697347137 ) ) ;
#13538 = CARTESIAN_POINT ( 'NONE',  ( 45.74753988029933538, 86.06518717409400665, 30.44471234641811819 ) ) ;
#13540 = CARTESIAN_POINT ( 'NONE',  ( -141.4692556286852891, -195.9891397928654726, 49.65701158161630957 ) ) ;
#13541 = CARTESIAN_POINT ( 'NONE',  ( -154.3824083646099439, -193.2938272943107449, 58.62277379824867296 ) ) ;
#13542 = CARTESIAN_POINT ( 'NONE',  ( 147.8787791192428074, -126.9891397928655010, 59.65701158161630957 ) ) ;
#13543 = CYLINDRICAL_SURFACE ( 'NONE', #6863, 4.999999999999997335 ) ;
#13544 = CARTESIAN_POINT ( 'NONE',  ( 44.55648932407425633, 142.6104996726487570, 38.96596240072933170 ) ) ;
#13545 = CARTESIAN_POINT ( 'NONE',  ( 47.43856463449117200, 149.0297705074273438, 32.77220824515698183 ) ) ;
#13546 = CARTESIAN_POINT ( 'NONE',  ( -143.9637021292201950, -126.9891397928655010, 62.65701158161630957 ) ) ;
#13547 = CARTESIAN_POINT ( 'NONE',  ( 48.17517050666977241, 153.7480039124125994, 4.005852979123367241 ) ) ;
#13548 = CARTESIAN_POINT ( 'NONE',  ( 43.01140435219951286, 143.3651871740940180, 29.55568802177586107 ) ) ;
#13549 = CARTESIAN_POINT ( 'NONE',  ( -142.0420953463935803, -165.5438272943107165, 52.72008163687743831 ) ) ;
#13550 = CARTESIAN_POINT ( 'NONE',  ( -157.2955611005345986, -178.7084106276440423, 57.67623309621197336 ) ) ;
#13551 = ADVANCED_FACE ( 'NONE', ( #3895 ), #14999, .T. ) ;
#13552 = EDGE_CURVE ( 'NONE', #18638, #9201, #4104, .T. ) ;
#13553 = CARTESIAN_POINT ( 'NONE',  ( 38.58424406990785371, 59.96518717409398391, 32.77220824515697473 ) ) ;
#13554 = CARTESIAN_POINT ( 'NONE',  ( -159.0959885057557983, -157.8584106276440480, 55.19815736654470584 ) ) ;
#13555 = CARTESIAN_POINT ( 'NONE',  ( 34.49559591455799534, 146.8750064778945728, 2.580435534661669195 ) ) ;
#13556 = CARTESIAN_POINT ( 'NONE',  ( 38.58424406990786082, 129.1151871740940180, 34.21067981925357060 ) ) ;
#13557 = VERTEX_POINT ( 'NONE', #19205 ) ;
#13558 = ORIENTED_EDGE ( 'NONE', *, *, #18980, .T. ) ;
#13559 = ORIENTED_EDGE ( 'NONE', *, *, #5607, .T. ) ;
#13560 = CARTESIAN_POINT ( 'NONE',  ( 48.01140435219951996, 103.1344580088725706, 35.83527830041810347 ) ) ;
#13561 = CARTESIAN_POINT ( 'NONE',  ( 39.42975644700377558, 153.6797705074273210, 36.81289934271958941 ) ) ;
#13562 = CARTESIAN_POINT ( 'NONE',  ( 46.59305225739526435, 70.57977050742732672, 36.81289934271958941 ) ) ;
#13564 = CARTESIAN_POINT ( 'NONE',  ( 52.12662541604375122, 146.5080492276505311, -15.72009227599853531 ) ) ;
#13563 = CARTESIAN_POINT ( 'NONE',  ( 39.42975644700377558, 116.8151871740940067, 31.60846029578754468 ) ) ;
#13565 = CARTESIAN_POINT ( 'NONE',  ( 46.10157429594899270, 82.76049967264874851, 38.46393386101376421 ) ) ;
#13566 = VECTOR ( 'NONE', #13621, 1000.000000000000000 ) ;
#13567 = CARTESIAN_POINT ( 'NONE',  ( 44.55648932407425633, 98.81049967264873146, 29.45539723777780239 ) ) ;
#13568 = CARTESIAN_POINT ( 'NONE',  ( 173.3794444120442506, -126.9891397928655010, -17.64809332337413750 ) ) ;
#13569 = CARTESIAN_POINT ( 'NONE',  ( 44.37947211624943833, 76.01518717409399528, 38.42115945441014446 ) ) ;
#13570 = CARTESIAN_POINT ( 'NONE',  ( 43.01140435219951286, 82.46049967264873715, 39.21067981925356349 ) ) ;
#13571 = CARTESIAN_POINT ( 'NONE',  ( 48.01140435219951996, 124.4344580088725536, 32.58608133808903773 ) ) ;
#13572 = CARTESIAN_POINT ( 'NONE',  ( 39.92123440845005433, 132.2604996726487343, 29.95742577749336988 ) ) ;
#13573 = EDGE_CURVE ( 'NONE', #11274, #784, #10516, .T. ) ;
#13574 = ORIENTED_EDGE ( 'NONE', *, *, #10434, .F. ) ;
#13575 = CARTESIAN_POINT ( 'NONE',  ( 44.37947211624943833, 65.47977050742731819, 30.00020018409699318 ) ) ;
#13576 =( BOUNDED_CURVE ( )  B_SPLINE_CURVE ( 2, ( #20261, #18605, #16718, #17151, #12085, #5153, #11981, #2067, #13630, #15295, #20368, #18491, #21807 ),
 .UNSPECIFIED., .F., .T. ) 
 B_SPLINE_CURVE_WITH_KNOTS ( ( 3, 2, 2, 2, 2, 2, 3 ),
 ( 0.3161764705882352811, 0.3176470588235293935, 0.3205882352941176738, 0.3235294117647058987, 0.3264705882352941235, 0.3294117647058823484, 0.3308823529411764608 ),
 .UNSPECIFIED. ) 
 CURVE ( )  GEOMETRIC_REPRESENTATION_ITEM ( )  RATIONAL_B_SPLINE_CURVE ( ( 0.9755282581475768211, 0.9755282581475768211, 1.000000000000000000, 0.9510565162951535312, 1.000000000000000000, 0.9510565162951535312, 1.000000000000000000, 0.9510565162951535312, 1.000000000000000000, 0.9510565162951535312, 1.000000000000000000, 0.9755282581475768211, 0.9755282581475768211 ) ) 
 REPRESENTATION_ITEM ( '' )  );
#13577 = CARTESIAN_POINT ( 'NONE',  ( -157.2955611005346270, -182.6084106276440480, 41.63779006702063867 ) ) ;
#13578 = CARTESIAN_POINT ( 'NONE',  ( 31.47436479266152531, 87.67613096727390598, 14.72005176623422606 ) ) ;
#13579 = CARTESIAN_POINT ( 'NONE',  ( -148.5561028927606344, -178.2584106276440536, 58.62277379824867296 ) ) ;
#13580 = ORIENTED_EDGE ( 'NONE', *, *, #9496, .F. ) ;
#13581 = CARTESIAN_POINT ( 'NONE',  ( 40.27526882409969033, 150.5651871740940067, 37.97664729208901946 ) ) ;
#13582 = CARTESIAN_POINT ( 'NONE',  ( 40.27526882409969744, 158.6651871740939725, 30.44471234641812174 ) ) ;
#13583 = CARTESIAN_POINT ( 'NONE',  ( 47.43856463449117911, 118.7297705074273040, 35.64915139335015937 ) ) ;
#13584 = CARTESIAN_POINT ( 'NONE',  ( 61.76154402333882132, 148.5480768402654803, 4.482004293238171400 ) ) ;
#13585 = VERTEX_POINT ( 'NONE', #4000 ) ;
#13586 =( NAMED_UNIT ( * ) PLANE_ANGLE_UNIT ( ) SI_UNIT ( $, .RADIAN. ) );
#13587 = ORIENTED_EDGE ( 'NONE', *, *, #12505, .T. ) ;
#13588 = CARTESIAN_POINT ( 'NONE',  ( 46.59305225739526435, 113.1797705074273210, 31.60846029578754468 ) ) ;
#13589 = DIRECTION ( 'NONE',  ( 0.000000000000000000, -1.000000000000000000, 0.000000000000000000 ) ) ;
#13590 = CARTESIAN_POINT ( 'NONE',  ( 43.01140435219951996, 10.71049967264875491, 39.21067981925356349 ) ) ;
#13591 = CARTESIAN_POINT ( 'NONE',  ( 46.59305225739526435, 85.57977050742732672, 36.81289934271958941 ) ) ;
#13592 = CARTESIAN_POINT ( 'NONE',  ( 43.01140435219951286, 156.8651871740940180, 38.86567161673127657 ) ) ;
#13593 = CARTESIAN_POINT ( 'NONE',  ( 34.64294707643933435, 153.0196542278736729, 4.557659493426334585 ) ) ;
#13594 = DIRECTION ( 'NONE',  ( -0.000000000000000000, -0.000000000000000000, -1.000000000000000000 ) ) ;
#13595 = FACE_OUTER_BOUND ( 'NONE', #19142, .T. ) ;
#13596 = CARTESIAN_POINT ( 'NONE',  ( -161.4692556286852607, -179.3391397928654953, 52.90620854394536821 ) ) ;
#13597 = DIRECTION ( 'NONE',  ( 1.000000000000000000, 0.000000000000000000, 0.000000000000000000 ) ) ;
#13598 = DIRECTION ( 'NONE',  ( 0.000000000000000000, 0.000000000000000000, -1.000000000000000000 ) ) ;
#13599 = CARTESIAN_POINT ( 'NONE',  ( 48.01140435219951996, 97.28445800887259054, 34.21067981925357060 ) ) ;
#13600 = VECTOR ( 'NONE', #17877, 1000.000000000000000 ) ;
#13601 = CIRCLE ( 'NONE', #1283, 4.999999999999997335 ) ;
#13602 = CARTESIAN_POINT ( 'NONE',  ( 43.01140435219951286, 94.12977050742730967, 38.86567161673127657 ) ) ;
#13603 = CARTESIAN_POINT ( 'NONE',  ( 18.86999673272213229, 105.3337293714367604, -5.438779171309367833 ) ) ;
#13604 = CARTESIAN_POINT ( 'NONE',  ( -159.0959885057557983, -176.1938272943107506, 44.11586579668791330 ) ) ;
#13605 = CARTESIAN_POINT ( 'NONE',  ( 43.01140435219951286, 78.86518717409400381, 38.86567161673127657 ) ) ;
#13606 = CARTESIAN_POINT ( 'NONE',  ( 163.1026836591718734, 192.4288937294299160, 34.00000000000001421 ) ) ;
#13607 = DIRECTION ( 'NONE',  ( 0.000000000000000000, 0.000000000000000000, 1.000000000000000000 ) ) ;
#13608 = VERTEX_POINT ( 'NONE', #9185 ) ;
#13609 = FACE_OUTER_BOUND ( 'NONE', #17446, .T. ) ;
#13610 = CARTESIAN_POINT ( 'NONE',  ( 47.05648932407426344, 121.9104996726487542, 37.14960608071593384 ) ) ;
#13611 = CARTESIAN_POINT ( 'NONE',  ( 28.48261614285185672, 95.83124311379776827, 2.017784757223194170 ) ) ;
#13612 = CARTESIAN_POINT ( 'NONE',  ( 40.27526882409969744, 59.92977050742730682, 30.44471234641812174 ) ) ;
#13613 = VERTEX_POINT ( 'NONE', #18994 ) ;
#13614 = VECTOR ( 'NONE', #21611, 1000.000000000000000 ) ;
#13615 = CARTESIAN_POINT ( 'NONE',  ( 43.01140435219951286, 134.6297705074273097, 29.55568802177586463 ) ) ;
#13616 = CARTESIAN_POINT ( 'NONE',  ( 44.37947211624943833, 100.2797705074273154, 38.42115945441014446 ) ) ;
#13617 = DIRECTION ( 'NONE',  ( -0.000000000000000000, 1.000000000000000000, -0.000000000000000000 ) ) ;
#13618 = CARTESIAN_POINT ( 'NONE',  ( 41.64333658814960870, 62.51518717409400239, 30.00020018409699318 ) ) ;
#13619 = DIRECTION ( 'NONE',  ( 0.000000000000000000, 1.000000000000000000, 0.000000000000000000 ) ) ;
#13620 = CARTESIAN_POINT ( 'NONE',  ( 38.01140435219952707, 153.5604996726487457, 32.58608133808903773 ) ) ;
#13621 = DIRECTION ( 'NONE',  ( 0.000000000000000000, 1.000000000000000000, 0.000000000000000000 ) ) ;
#13622 = CARTESIAN_POINT ( 'NONE',  ( -141.4692556286852891, -165.0630981290893260, 49.65701158161630957 ) ) ;
#13623 = DIRECTION ( 'NONE',  ( 0.9820818503191364179, -6.938893903907228378E-18, -0.1884548733085491812 ) ) ;
#13624 = CARTESIAN_POINT ( 'NONE',  ( 48.01140435219951996, 139.4344580088725252, 32.58608133808903773 ) ) ;
#13625 = CARTESIAN_POINT ( 'NONE',  ( 39.42975644700377558, 123.0797705074273267, 31.60846029578754468 ) ) ;
#13626 = CARTESIAN_POINT ( 'NONE',  ( 12.26432857192422432, 135.0705202968918570, 22.59931835930844457 ) ) ;
#13627 = CARTESIAN_POINT ( 'NONE',  ( 30.18028515090310293, 151.2280014487710957, 17.43780275515693390 ) ) ;
#13628 = AXIS2_PLACEMENT_3D ( 'NONE', #3920, #10867, #17352 ) ;
#13629 = CARTESIAN_POINT ( 'NONE',  ( 46.59305225739526435, 109.3151871740939924, 36.81289934271958941 ) ) ;
#13630 = CARTESIAN_POINT ( 'NONE',  ( 38.96631938032478359, 125.4844580088725934, 31.27175355779120025 ) ) ;
#13631 = EDGE_CURVE ( 'NONE', #5984, #19572, #19244, .T. ) ;
#13632 = CARTESIAN_POINT ( 'NONE',  ( 66.03587854725165585, 94.68079322629401418, 0.5104136635535641009 ) ) ;
#13633 = CARTESIAN_POINT ( 'NONE',  ( 66.49460585200260709, 135.5194395740885511, -1.986604139701473759 ) ) ;
#13634 = CARTESIAN_POINT ( 'NONE',  ( -148.3790856849358306, -155.4630981290893033, 40.14644641866477315 ) ) ;
#13635 = CARTESIAN_POINT ( 'NONE',  ( 43.01140435219951286, 89.62977050742730967, 29.55568802177586107 ) ) ;
#13636 =( BOUNDED_CURVE ( )  B_SPLINE_CURVE ( 2, ( #12369, #20867, #9190, #12049, #2450, #18999, #8758, #376, #7105, #20548, #4108, #2342, #10844 ),
 .UNSPECIFIED., .F., .F. ) 
 B_SPLINE_CURVE_WITH_KNOTS ( ( 3, 2, 2, 2, 2, 2, 3 ),
 ( 0.3392857142857142461, 0.3428571428571428603, 0.3499999999999999778, 0.3571428571428571508, 0.3642857142857142683, 0.3714285714285714413, 0.3750000000000000000 ),
 .UNSPECIFIED. ) 
 CURVE ( )  GEOMETRIC_REPRESENTATION_ITEM ( )  RATIONAL_B_SPLINE_CURVE ( ( 0.9755282581475768211, 0.9755282581475765991, 1.000000000000000000, 0.9510565162951535312, 1.000000000000000000, 0.9510565162951535312, 1.000000000000000000, 0.9510565162951535312, 1.000000000000000000, 0.9510565162951535312, 1.000000000000000000, 0.9755282581475768211, 0.9755282581475768211 ) ) 
 REPRESENTATION_ITEM ( '' )  );
#13637 = ORIENTED_EDGE ( 'NONE', *, *, #5906, .F. ) ;
#13638 = AXIS2_PLACEMENT_3D ( 'NONE', #5206, #11922, #18651 ) ;
#13639 = DIRECTION ( 'NONE',  ( -0.000000000000000000, 1.000000000000000000, -0.000000000000000000 ) ) ;
#13640 = CARTESIAN_POINT ( 'NONE',  ( 41.46631938032478359, 72.38445800887258486, 38.96596240072933170 ) ) ;
#13641 = CARTESIAN_POINT ( 'NONE',  ( 38.01140435219952707, 59.93445800887258201, 35.83527830041809636 ) ) ;
#13642 = VECTOR ( 'NONE', #4963, 1000.000000000000000 ) ;
#13644 = EDGE_CURVE ( 'NONE', #20857, #18306, #8966, .T. ) ;
#13643 = CARTESIAN_POINT ( 'NONE',  ( 38.96631938032478359, 132.4104996726487684, 31.27175355779120025 ) ) ;
#13646 = CARTESIAN_POINT ( 'NONE',  ( 54.88857506304572809, 87.88569651147935247, -13.06129575545291210 ) ) ;
#13645 = CARTESIAN_POINT ( 'NONE',  ( 46.59305225739526435, 85.31518717409400665, 36.81289934271958941 ) ) ;
#13647 = CARTESIAN_POINT ( 'NONE',  ( -148.5561028927606344, -157.2584106276440536, 58.62277379824867296 ) ) ;
#13648 = CARTESIAN_POINT ( 'NONE',  ( -157.2955611005345986, -181.4438272943107506, 57.67623309621197336 ) ) ;
#13649 = CARTESIAN_POINT ( 'NONE',  ( 41.46631938032478359, 93.11049967264874283, 29.45539723777780239 ) ) ;
#13650 = DIRECTION ( 'NONE',  ( -0.7067093775913396714, 0.7073806645723093034, -0.01320799052465169467 ) ) ;
#13651 = FACE_OUTER_BOUND ( 'NONE', #14873, .T. ) ;
#13652 = CARTESIAN_POINT ( 'NONE',  ( 116.9721770337685740, 160.7104996726487514, -25.00000000000000000 ) ) ;
#13653 = CARTESIAN_POINT ( 'NONE',  ( 40.27526882409969033, 155.9297705074273210, 30.44471234641811819 ) ) ;
#13654 = CARTESIAN_POINT ( 'NONE',  ( 44.37947211624943833, 103.2797705074273154, 38.42115945441014446 ) ) ;
#13655 = EDGE_CURVE ( 'NONE', #13229, #1905, #11129, .T. ) ;
#13656 = CARTESIAN_POINT ( 'NONE',  ( 32.07966263401961982, 152.4337125855422528, -4.522337938825778281 ) ) ;
#13657 = CARTESIAN_POINT ( 'NONE',  ( 47.43856463449117911, 142.4651871740940123, 35.64915139335015937 ) ) ;
#13658 = CARTESIAN_POINT ( 'NONE',  ( 173.3794444120442506, 0.000000000000000000, 30.00000000000000000 ) ) ;
#13659 = CARTESIAN_POINT ( 'NONE',  ( -142.0420953463936087, -171.6584106276440593, 49.65701158161630957 ) ) ;
#13660 = CARTESIAN_POINT ( 'NONE',  ( 43.01140435219951286, 62.36518717409398960, 29.55568802177586107 ) ) ;
#13661 = CARTESIAN_POINT ( 'NONE',  ( -160.8964159109769696, -158.3084106276440650, 46.59394152635518793 ) ) ;
#13662 = CARTESIAN_POINT ( 'NONE',  ( 35.43645570112151688, 92.65990651318493576, -0.2767073223962682738 ) ) ;
#13663 = EDGE_CURVE ( 'NONE', #16995, #12027, #10727, .T. ) ;
#13664 = PRESENTATION_STYLE_ASSIGNMENT (( #5292 ) ) ;
#13665 = CARTESIAN_POINT ( 'NONE',  ( 45.74753988029933538, 118.1651871740939725, 37.97664729208901946 ) ) ;
#13666 = ORIENTED_EDGE ( 'NONE', *, *, #12147, .F. ) ;
#13667 = VERTEX_POINT ( 'NONE', #8071 ) ;
#13668 = CARTESIAN_POINT ( 'NONE',  ( 41.46631938032478359, 113.1844580088725820, 29.45539723777780239 ) ) ;
#13669 = ORIENTED_EDGE ( 'NONE', *, *, #17350, .F. ) ;
#13670 = CARTESIAN_POINT ( 'NONE',  ( 39.92123440845004723, 104.3344580088725735, 29.95742577749337343 ) ) ;
#13671 = DIRECTION ( 'NONE',  ( -0.5010362705417045204, -0.000000000000000000, 0.8654262854811263228 ) ) ;
#13672 = CARTESIAN_POINT ( 'NONE',  ( 41.64333658814960870, 60.97977050742731109, 38.42115945441014446 ) ) ;
#13674 = CARTESIAN_POINT ( 'NONE',  ( 71.10646316465144423, 118.7373161137383732, -14.29152813157908319 ) ) ;
#13673 = CARTESIAN_POINT ( 'NONE',  ( 39.42975644700377558, 114.4151871740940010, 36.81289934271958941 ) ) ;
#13675 = CARTESIAN_POINT ( 'NONE',  ( 48.01140435219951996, 77.06049967264874567, 35.83527830041810347 ) ) ;
#13676 = CARTESIAN_POINT ( 'NONE',  ( 147.8787791192428074, -126.9891397928655010, 59.65701158161630957 ) ) ;
#13677 = ADVANCED_FACE ( 'NONE', ( #13133, #4313, #14450 ), #19637, .T. ) ;
#13678 = CARTESIAN_POINT ( 'NONE',  ( 39.92123440845005433, 71.33445800887257349, 29.95742577749336988 ) ) ;
#13679 = CARTESIAN_POINT ( 'NONE',  ( 44.30846152966199725, 94.93869211110843764, 39.05053369627938054 ) ) ;
#13680 = CARTESIAN_POINT ( 'NONE',  ( 43.01140435219951286, 75.86518717409398960, 38.86567161673127657 ) ) ;
#13681 = DIRECTION ( 'NONE',  ( 1.000000000000000000, 0.000000000000000000, 0.000000000000000000 ) ) ;
#13682 = CARTESIAN_POINT ( 'NONE',  ( -160.8964159109769696, -179.0438272943107449, 46.59394152635518793 ) ) ;
#13683 = CARTESIAN_POINT ( 'NONE',  ( 147.8787791192428074, -136.9891397928655010, 39.65701158161628825 ) ) ;
#13684 = ORIENTED_EDGE ( 'NONE', *, *, #10273, .F. ) ;
#13685 = CARTESIAN_POINT ( 'NONE',  ( -159.0959885057557983, -185.4584106276440707, 44.11586579668791330 ) ) ;
#13686 = CARTESIAN_POINT ( 'NONE',  ( 11.08170843061617816, 132.1625483722078513, 16.49545033792581350 ) ) ;
#13687 = CARTESIAN_POINT ( 'NONE',  ( -160.8964159109769696, -173.0084106276440821, 52.72008163687743121 ) ) ;
#13688 = ORIENTED_EDGE ( 'NONE', *, *, #719, .T. ) ;
#13689 = CARTESIAN_POINT ( 'NONE',  ( 38.58424406990784661, 155.9651871740939555, 32.77220824515698183 ) ) ;
#13690 = CARTESIAN_POINT ( 'NONE',  ( 43.01140435219951286, 158.3651871740939896, 29.55568802177586107 ) ) ;
#13691 = ADVANCED_FACE ( 'NONE', ( #1338 ), #16318, .T. ) ;
#13692 = CARTESIAN_POINT ( 'NONE',  ( 47.43856463449117911, 116.0297705074273296, 32.77220824515697473 ) ) ;
#13693 = CARTESIAN_POINT ( 'NONE',  ( 37.24990543953586553, 153.6521207556136517, 3.648881909465930828 ) ) ;
#13694 = ORIENTED_EDGE ( 'NONE', *, *, #5607, .F. ) ;
#13695 = VECTOR ( 'NONE', #18050, 1000.000000000000000 ) ;
#13696 =( NAMED_UNIT ( * ) SI_UNIT ( $, .STERADIAN. ) SOLID_ANGLE_UNIT ( ) );
#13697 = ORIENTED_EDGE ( 'NONE', *, *, #14599, .T. ) ;
#13698 = CARTESIAN_POINT ( 'NONE',  ( 43.01140435219951996, 10.71049967264875491, 29.21067981925357060 ) ) ;
#13699 = CARTESIAN_POINT ( 'NONE',  ( 43.01140435219951286, 129.5344580088725763, 39.21067981925356349 ) ) ;
#13700 = CARTESIAN_POINT ( 'NONE',  ( 46.59305225739526435, 148.9151871740940294, 31.60846029578754468 ) ) ;
#13701 = CARTESIAN_POINT ( 'NONE',  ( 9.616596702810701558, 112.3753283828585694, -5.161025107254184618 ) ) ;
#13702 = CARTESIAN_POINT ( 'NONE',  ( 48.01140435219951996, 82.13445800887255643, 35.83527830041809636 ) ) ;
#13703 = DIRECTION ( 'NONE',  ( 0.9385982292947087080, 0.3450121214752279175, 0.000000000000000000 ) ) ;
#13704 = CARTESIAN_POINT ( 'NONE',  ( -143.3790856849358306, -169.2891397928654840, 55.53486410454105027 ) ) ;
#13705 =( BOUNDED_SURFACE ( )  B_SPLINE_SURFACE ( 3, 3, ( 
 ( #15975, #2755, #19297, #7625, #4295, #7943, #17953, #19616, #14326, #19505, #481, #6161, #14216, #6277, #4511, #5839, #9495, #11234, #13009, #21282, #2859, #21068, #12570, #16193, #4195, #2537, #2137, #12677, #15577, #1104, #10923, #10524, #11131, #17220, #8869, #7839, #11022, #16086, #17846, #9602, #12896, #996, #17630, #7734, #14435, #16302, #21169, #6059, #12785, #4398, #10146, #21614, #16633, #6739, #19962, #18065, #11451, #18409, #16517, #16848, #3085, #18296, #6624, #18179, #1544, #13339, #9710, #4732, #11674, #2132, #13446, #15209, #20076, #1763, #8055, #6391, #11786, #4846, #6504, #14975, #109, #9819, #13118, #11342, #8163, #13547, #8497, #14869, #19841, #1433, #18516, #1653, #6841, #13224, #4622, #11567, #2971, #16412, #3198, #20181, #8385, #5072, #16742, #1321, #14761, #3426, #21503, #9928, #15094, #3309, #8275, #21721, #4964, #10038, #7273, #5596, #20713, #13975, #12106, #18838, #3961, #15629, #3638, #9032, #1977, #7383, #10363, #2193, #18625, #20283, #5489, #10255, #17279, #326, #5390, #5178, #3744, #12216, #16957, #8924, #18950, #20389, #10474, #534, #17174, #12323, #19058, #10683, #17388, #2087, #8820, #2292, #15743, #17064, #648, #8711, #11896, #15430, #3530, #1869, #8599, #3851 ),
 ( #15529, #15319, #212, #6949, #13656, #5286, #12000, #18733, #7056, #13761, #20501, #434, #7165, #13868, #20606, #19481, #2407, #5812, #5711, #19271, #19162, #4372, #15843, #2834, #14409, #11209, #4481, #11103, #9251, #12543, #21145, #7811, #6030, #861, #1185, #17925, #4271, #14517, #16168, #7598, #12760, #9573, #19588, #14297, #10999, #1080, #21041, #12436, #20931, #17816, #4171, #16279, #10900, #5924, #16057, #17604, #17709, #968, #4061, #14191, #2729, #9469, #21257, #20820, #7709, #10790, #17496, #754, #6137, #12652, #19376, #2614, #9143, #2510, #7489, #9352, #12869, #16824, #20153, #11422, #9685, #1294, #15066, #4936, #5045, #9795, #11756, #6363, #18487, #3393, #21472, #3279, #11646, #10009, #20049, #10117, #11314, #16714, #7919, #13087, #1623, #18378, #8355, #21803, #14622, #18038, #6711, #21359, #19704, #13418, #6594, #8029, #21584, #6250, #6474, #12980, #4595, #2943, #16382, #13195, #19928, #14736, #19815, #4704, #18148, #3055, #16488, #1405, #8134, #14837, #4816, #14948, #11539, #18266, #3170, #9899, #16601, #1517, #21695, #8247, #13313, #5150, #13949, #17252, #13524, #409, #10551, #3930, #5465, #15604, #6922, #3505, #7139, #11869, #15292, #15179, #13626, #6818, #13843, #10228, #12294, #2064 ),
 ( #20687, #19032, #512, #7249, #5571, #5365, #10661, #5260, #3614, #20579, #20365, #15507, #16930, #11977, #17039, #1736, #8902, #2165, #18707, #10446, #8471, #12082, #301, #18812, #1846, #20258, #18601, #8681, #10336, #3825, #12187, #18922, #7030, #8576, #81, #15403, #185, #1951, #3717, #13735, #20473, #17148, #8793, #1052, #4038, #16027, #7786, #16144, #17686, #19245, #14382, #19139, #9328, #10765, #12520, #2484, #19349, #17471, #2381, #9119, #12734, #17578, #4144, #14490, #15817, #940, #21232, #6111, #2588, #10877, #21121, #731, #7685, #7459, #9226, #15924, #4247, #14168, #20901, #5788, #12841, #836, #7570, #9443, #14270, #15717, #2269, #21015, #10973, #5897, #12627, #11075, #19559, #6005, #4454, #19457, #4347, #17790, #17363, #2698, #9006, #621, #7356, #14059, #20793, #5685, #12408, #6686, #11512, #6337, #14814, #21672, #4682, #18121, #18012, #9549, #12954, #1492, #6567, #16465, #13063, #14923, #2811, #4569, #9658, #11624, #13287, #21559, #18352, #19677, #11185, #1269, #21447, #9986, #19790, #11291, #16252, #16573, #8108, #20022, #1597, #3143, #19903, #4908, #1161, #17898, #8004, #8330, #15039, #13394, #3256, #16689, #21780, #6449, #20128, #14711, #11397, #8222, #16358, #9873, #2923, #3031 ),
 ( #9768, #7894, #1379, #13171, #4791, #18241, #14596, #21336, #6223, #6795, #8657, #5338, #12055, #13816, #10312, #382, #1712, #15152, #17122, #15266, #11845, #15379, #53, #18574, #8554, #7111, #2034, #18786, #3481, #17014, #3689, #18682, #13603, #3584, #13502, #16799, #8447, #163, #10205, #10417, #20446, #13710, #20340, #10092, #20556, #6896, #272, #20234, #1921, #16908, #8766, #5235, #1820, #15481, #5127, #7006, #5439, #5022, #11731, #11952, #18464, #3367, #16652, #18085, #19863, #9838, #4867, #2991, #9732, #16429, #17, #11470, #1341, #16762, #14888, #1230, #9622, #16538, #11588, #4750, #14781, #18429, #5091, #11364, #8405, #8075, #6648, #21524, #15114, #1454, #11694, #3327, #8187, #1673, #6299, #16321, #21411, #20198, #3216, #18199, #6525, #13357, #3106, #21634, #6413, #7964, #4646, #14998, #20094, #13246, #19982, #4983, #14671, #13136, #18316, #10056, #6757, #9949, #13465, #1564, #2883, #8291, #21740, #11805, #13028, #19752, #1783, #2101, #15445, #5506, #8941, #10489, #5404, #20623, #10168, #3443, #15338, #15647, #551, #13994, #10593, #2210, #17298, #346, #5618, #230, #20407, #8839, #12236, #3870, #18967, #7295, #10382, #17082, #20730, #13884, #1885, #18536, #6968, #16869, #8619, #450 ),
 ( #5305, #3654, #8517, #1996, #17189, #15230, #128, #6857, #13564, #20300, #5198, #15545, #11915, #18645, #7180, #3547, #13674, #10272, #16975, #12017, #18751, #8727, #7075, #13778, #20517, #12121, #18854, #3762, #9486, #2747, #9371, #7508, #10810, #12671, #6051, #19391, #14208, #21274, #16185, #2530, #12777, #14427, #20947, #4288, #1097, #17837, #5829, #9266, #21162, #12562, #3977, #19181, #11015, #2422, #7831, #17513, #4188, #14317, #4080, #15966, #21060, #17406, #12453, #17726, #7725, #19498, #14533, #5941, #12341, #15759, #14102, #4390, #19289, #10916, #878, #19076, #9162, #20838, #10702, #15861, #2311, #9050, #774, #5729, #17622, #11122, #16076, #664, #7615, #7401, #2631, #987, #10026, #19720, #1532, #9915, #8264, #18285, #16731, #9593, #14964, #1641, #17943, #16622, #4834, #6266, #19830, #21711, #4720, #16294, #4611, #19608, #11332, #11224, #11557, #7935, #8374, #6492, #3298, #18398, #3187, #1311, #18053, #13212, #6614, #19949, #8046, #15084, #6152, #18165, #13330, #20066, #14751, #4953, #12887, #11661, #21492, #3073, #4501, #6378, #2849, #12999, #1200, #2961, #14639, #9700, #11440, #8152, #16400, #9811, #14857, #21380, #13107, #16506, #1423, #21603, #10568, #1967, #18941, #3414, #1754, #7155 ),
 ( #8489, #20490, #5481, #20595, #7045, #1860, #18828, #15198, #5380, #101, #16944, #6939, #8700, #6832, #13539, #20274, #3841, #8590, #5166, #13858, #11991, #20173, #6729, #13646, #15421, #15309, #11887, #15520, #2180, #18615, #12206, #3520, #3733, #10246, #17269, #20380, #8809, #423, #18721, #15495, #10137, #13435, #18505, #5063, #12095, #201, #3628, #10463, #10352, #17055, #17164, #11776, #2078, #16841, #4264, #20921, #17488, #19366, #7264, #9023, #14075, #16048, #10992, #19262, #959, #17378, #15619, #5703, #4054, #14400, #2718, #19473, #5804, #9345, #17702, #2398, #853, #4365, #21138, #10782, #12535, #2607, #9135, #13965, #639, #7589, #12427, #6022, #20813, #7481, #17596, #7374, #4164, #2502, #20705, #15734, #14289, #7702, #12753, #11095, #9244, #17807, #19049, #2283, #527, #15835, #746, #10893, #5588, #19153, #14183, #12313, #15943, #3949, #10675, #21033, #5916, #12645, #16897, #6784, #6886, #11615, #13593, #8213, #20331, #5228, #1176, #5117, #13493, #11835, #44, #11943, #12858, #18565, #18673, #21250, #20225, #8433, #9565, #1589, #3471, #8320, #10195, #1811, #8543, #15255, #15030, #21770, #154, #9459, #14912, #16160, #13277, #1072, #21662, #7802, #14508, #6128, #16791, #19579, #4472, #18343 ),
 ( #11202, #17915, #2825, #16270, #6552, #15141, #20012, #4896, #3244, #9975, #16679, #6675, #13382, #20120, #5011, #11720, #18455, #3356, #10081, #1704, #14127, #3898, #691, #15785, #580, #20547, #2027, #10622, #19107, #17330, #5430, #20652, #12048, #262, #13701, #10520, #15474, #5648, #14023, #7323, #2130, #15369, #20866, #17215, #8971, #6997, #5535, #8757, #20757, #3791, #12150, #9078, #18778, #2237, #7428, #2341, #15676, #18882, #12368, #5330, #4003, #3681, #8865, #15573, #12263, #10409, #17111, #374, #5753, #477, #7104, #17433, #7213, #1911, #10301, #13913, #18998, #10732, #13809, #12483, #3575, #17004, #8647, #20436, #1127, #4214, #2886, #4317, #6187, #12918, #2659, #17975, #800, #4107, #15887, #14673, #4421, #14349, #1019, #7861, #12698, #11041, #10943, #17539, #20976, #9518, #14561, #9403, #21090, #21303, #10843, #12595, #17650, #19643, #4534, #14454, #11254, #5864, #19210, #9294, #7650, #9624, #5971, #19316, #2449, #2778, #16113, #16323, #1232, #11151, #12807, #7966, #9189, #7534, #15995, #21414, #6302, #14236, #2557, #904, #19420, #21193, #17757, #17866, #16217, #18431, #18201, #4986, #21526, #3108, #6528, #10171, #20200, #19, #9840, #21743, #6759, #1567, #11590, #19867, #11696, #16540 ) ),
 .UNSPECIFIED., .T., .F., .F. ) 
 B_SPLINE_SURFACE_WITH_KNOTS ( ( 4, 3, 4 ),
 ( 4, 2, 2, 2, 2, 2, 2, 2, 2, 2, 2, 2, 2, 2, 2, 2, 2, 2, 2, 2, 2, 2, 2, 2, 2, 2, 2, 2, 2, 2, 2, 2, 2, 2, 2, 2, 2, 2, 2, 2, 2, 2, 2, 2, 2, 2, 2, 2, 2, 2, 2, 2, 2, 2, 2, 2, 2, 2, 2, 2, 2, 2, 2, 2, 2, 2, 2, 2, 2, 2, 2, 2, 2, 2, 2, 2, 2, 2, 2, 2, 4 ),
 ( 0.000000000000000000, 0.5000000000000000000, 1.000000000000000000 ),
 ( 0.000000000000000000, 0.008318061648474830982, 0.01871563870907547167, 0.02911321576967611582, 0.03951079283027675998, 0.04990836989087740067, 0.06030594695147804829, 0.07070352401207868898, 0.08110110107267932966, 0.09149867813327997035, 0.1018962551938805972, 0.1122938322544812378, 0.1226914093150818785, 0.1330889863756825053, 0.1434865634362831321, 0.1538841404968837590, 0.1642817175574843858, 0.1746792946180850126, 0.1850768716786856394, 0.1954744487392862939, 0.2058720257998869485, 0.2162696028604875753, 0.2266671799210882021, 0.2370647569816888289, 0.2474623340422894557, 0.2578599111028900825, 0.2682574881634907094, 0.2786550652240913362, 0.2890526422846919630, 0.2994502193452925343, 0.3098477964058931611, 0.3202453734664937879, 0.3306429505270944147, 0.3410405275876950415, 0.3514381046482956683, 0.3618356817088962951, 0.3722332587694969219, 0.3826308358300975487, 0.3930284128906983421, 0.4034259899512990799, 0.4138235670118998732, 0.4242211440725006666, 0.4346187211331002942, 0.4450162981936999218, 0.4554138752542995494, 0.4658114523148991770, 0.4762090293755006920, 0.4866066064361021515, 0.4970041834967036110, 0.5074017605573051259, 0.5177993376179057528, 0.5281969146785063796, 0.5385944917391070064, 0.5489920687997077442, 0.5593896458603083710, 0.5697872229209089978, 0.5801847999815096246, 0.5905823770421102514, 0.6009799541027108782, 0.6113775311633115050, 0.6217751082239121319, 0.6321726852845127587, 0.6425702623451133855, 0.6529678394057140123, 0.6633654164663146391, 0.6737629935269152659, 0.6841605705875142274, 0.6945581476481130778, 0.7049557247087120393, 0.7153533017693110008, 0.7257508788299132929, 0.7361484558905155851, 0.7465460329511179882, 0.7569436100117202804, 0.7673411870723210182, 0.7777387641329216450, 0.7881363411935222718, 0.7985339182541228986, 0.8080132075800156022, 0.8174924969059083057, 0.8280181261579530050 ),
 .UNSPECIFIED. ) 
 GEOMETRIC_REPRESENTATION_ITEM ( )  RATIONAL_B_SPLINE_SURFACE ( (
 ( 1.000000000000000000, 1.000000000000000000, 1.000000000000000000, 1.000000000000000000, 1.000000000000000000, 1.000000000000000000, 1.000000000000000000, 1.000000000000000000, 1.000000000000000000, 1.000000000000000000, 1.000000000000000000, 1.000000000000000000, 1.000000000000000000, 1.000000000000000000, 1.000000000000000000, 1.000000000000000000, 1.000000000000000000, 1.000000000000000000, 1.000000000000000000, 1.000000000000000000, 1.000000000000000000, 1.000000000000000000, 1.000000000000000000, 1.000000000000000000, 1.000000000000000000, 1.000000000000000000, 1.000000000000000000, 1.000000000000000000, 1.000000000000000000, 1.000000000000000000, 1.000000000000000000, 1.000000000000000000, 1.000000000000000000, 1.000000000000000000, 1.000000000000000000, 1.000000000000000000, 1.000000000000000000, 1.000000000000000000, 1.000000000000000000, 1.000000000000000000, 1.000000000000000000, 1.000000000000000000, 1.000000000000000000, 1.000000000000000000, 1.000000000000000000, 1.000000000000000000, 1.000000000000000000, 1.000000000000000000, 1.000000000000000000, 1.000000000000000000, 1.000000000000000000, 1.000000000000000000, 1.000000000000000000, 1.000000000000000000, 1.000000000000000000, 1.000000000000000000, 1.000000000000000000, 1.000000000000000000, 1.000000000000000000, 1.000000000000000000, 1.000000000000000000, 1.000000000000000000, 1.000000000000000000, 1.000000000000000000, 1.000000000000000000, 1.000000000000000000, 1.000000000000000000, 1.000000000000000000, 1.000000000000000000, 1.000000000000000000, 1.000000000000000000, 1.000000000000000000, 1.000000000000000000, 1.000000000000000000, 1.000000000000000000, 1.000000000000000000, 1.000000000000000000, 1.000000000000000000, 1.000000000000000000, 1.000000000000000000, 1.000000000000000000, 1.000000000000000000, 1.000000000000000000, 1.000000000000000000, 1.000000000000000000, 1.000000000000000000, 1.000000000000000000, 1.000000000000000000, 1.000000000000000000, 1.000000000000000000, 1.000000000000000000, 1.000000000000000000, 1.000000000000000000, 1.000000000000000000, 1.000000000000000000, 1.000000000000000000, 1.000000000000000000, 1.000000000000000000, 1.000000000000000000, 1.000000000000000000, 1.000000000000000000, 1.000000000000000000, 1.000000000000000000, 1.000000000000000000, 1.000000000000000000, 1.000000000000000000, 1.000000000000000000, 1.000000000000000000, 1.000000000000000000, 1.000000000000000000, 1.000000000000000000, 1.000000000000000000, 1.000000000000000000, 1.000000000000000000, 1.000000000000000000, 1.000000000000000000, 1.000000000000000000, 1.000000000000000000, 1.000000000000000000, 1.000000000000000000, 1.000000000000000000, 1.000000000000000000, 1.000000000000000000, 1.000000000000000000, 1.000000000000000000, 1.000000000000000000, 1.000000000000000000, 1.000000000000000000, 1.000000000000000000, 1.000000000000000000, 1.000000000000000000, 1.000000000000000000, 1.000000000000000000, 1.000000000000000000, 1.000000000000000000, 1.000000000000000000, 1.000000000000000000, 1.000000000000000000, 1.000000000000000000, 1.000000000000000000, 1.000000000000000000, 1.000000000000000000, 1.000000000000000000, 1.000000000000000000, 1.000000000000000000, 1.000000000000000000, 1.000000000000000000, 1.000000000000000000, 1.000000000000000000, 1.000000000000000000, 1.000000000000000000, 1.000000000000000000, 1.000000000000000000, 1.000000000000000000, 1.000000000000000000, 1.000000000000000000, 1.000000000000000000, 1.000000000000000000, 1.000000000000000000, 1.000000000000000000, 1.000000000000000000, 1.000000000000000000),
 ( 0.3333333333333333703, 0.3333333333333333703, 0.3333333333333333703, 0.3333333333333333703, 0.3333333333333333703, 0.3333333333333333703, 0.3333333333333333703, 0.3333333333333333703, 0.3333333333333333703, 0.3333333333333333703, 0.3333333333333333703, 0.3333333333333333703, 0.3333333333333333703, 0.3333333333333333703, 0.3333333333333333703, 0.3333333333333333703, 0.3333333333333333703, 0.3333333333333333703, 0.3333333333333333703, 0.3333333333333333703, 0.3333333333333333703, 0.3333333333333333703, 0.3333333333333333703, 0.3333333333333333703, 0.3333333333333333703, 0.3333333333333333703, 0.3333333333333333703, 0.3333333333333333703, 0.3333333333333333703, 0.3333333333333333703, 0.3333333333333333703, 0.3333333333333333703, 0.3333333333333333703, 0.3333333333333333703, 0.3333333333333333703, 0.3333333333333333703, 0.3333333333333333703, 0.3333333333333333703, 0.3333333333333333703, 0.3333333333333333703, 0.3333333333333333703, 0.3333333333333333703, 0.3333333333333333703, 0.3333333333333333703, 0.3333333333333333703, 0.3333333333333333703, 0.3333333333333333703, 0.3333333333333333703, 0.3333333333333333703, 0.3333333333333333703, 0.3333333333333333703, 0.3333333333333333703, 0.3333333333333333703, 0.3333333333333333703, 0.3333333333333333703, 0.3333333333333333703, 0.3333333333333333703, 0.3333333333333333703, 0.3333333333333333703, 0.3333333333333333703, 0.3333333333333333703, 0.3333333333333333703, 0.3333333333333333703, 0.3333333333333333703, 0.3333333333333333703, 0.3333333333333333703, 0.3333333333333333703, 0.3333333333333333703, 0.3333333333333333703, 0.3333333333333333703, 0.3333333333333333703, 0.3333333333333333703, 0.3333333333333333703, 0.3333333333333333703, 0.3333333333333333703, 0.3333333333333333703, 0.3333333333333333703, 0.3333333333333333703, 0.3333333333333333703, 0.3333333333333333703, 0.3333333333333333703, 0.3333333333333333703, 0.3333333333333333703, 0.3333333333333333703, 0.3333333333333333703, 0.3333333333333333703, 0.3333333333333333703, 0.3333333333333333703, 0.3333333333333333703, 0.3333333333333333703, 0.3333333333333333703, 0.3333333333333333703, 0.3333333333333333703, 0.3333333333333333703, 0.3333333333333333703, 0.3333333333333333703, 0.3333333333333333703, 0.3333333333333333703, 0.3333333333333333703, 0.3333333333333333703, 0.3333333333333333703, 0.3333333333333333703, 0.3333333333333333703, 0.3333333333333333703, 0.3333333333333333703, 0.3333333333333333703, 0.3333333333333333703, 0.3333333333333333703, 0.3333333333333333703, 0.3333333333333333703, 0.3333333333333333703, 0.3333333333333333703, 0.3333333333333333703, 0.3333333333333333703, 0.3333333333333333703, 0.3333333333333333703, 0.3333333333333333703, 0.3333333333333333703, 0.3333333333333333703, 0.3333333333333333703, 0.3333333333333333703, 0.3333333333333333703, 0.3333333333333333703, 0.3333333333333333703, 0.3333333333333333703, 0.3333333333333333703, 0.3333333333333333703, 0.3333333333333333703, 0.3333333333333333703, 0.3333333333333333703, 0.3333333333333333703, 0.3333333333333333703, 0.3333333333333333703, 0.3333333333333333703, 0.3333333333333333703, 0.3333333333333333703, 0.3333333333333333703, 0.3333333333333333703, 0.3333333333333333703, 0.3333333333333333703, 0.3333333333333333703, 0.3333333333333333703, 0.3333333333333333703, 0.3333333333333333703, 0.3333333333333333703, 0.3333333333333333703, 0.3333333333333333703, 0.3333333333333333703, 0.3333333333333333703, 0.3333333333333333703, 0.3333333333333333703, 0.3333333333333333703, 0.3333333333333333703, 0.3333333333333333703, 0.3333333333333333703, 0.3333333333333333703, 0.3333333333333333703, 0.3333333333333333703, 0.3333333333333333703, 0.3333333333333333703, 0.3333333333333333703, 0.3333333333333333703),
 ( 0.3333333333333333703, 0.3333333333333333703, 0.3333333333333333703, 0.3333333333333333703, 0.3333333333333333703, 0.3333333333333333703, 0.3333333333333333703, 0.3333333333333333703, 0.3333333333333333703, 0.3333333333333333703, 0.3333333333333333703, 0.3333333333333333703, 0.3333333333333333703, 0.3333333333333333703, 0.3333333333333333703, 0.3333333333333333703, 0.3333333333333333703, 0.3333333333333333703, 0.3333333333333333703, 0.3333333333333333703, 0.3333333333333333703, 0.3333333333333333703, 0.3333333333333333703, 0.3333333333333333703, 0.3333333333333333703, 0.3333333333333333703, 0.3333333333333333703, 0.3333333333333333703, 0.3333333333333333703, 0.3333333333333333703, 0.3333333333333333703, 0.3333333333333333703, 0.3333333333333333703, 0.3333333333333333703, 0.3333333333333333703, 0.3333333333333333703, 0.3333333333333333703, 0.3333333333333333703, 0.3333333333333333703, 0.3333333333333333703, 0.3333333333333333703, 0.3333333333333333703, 0.3333333333333333703, 0.3333333333333333703, 0.3333333333333333703, 0.3333333333333333703, 0.3333333333333333703, 0.3333333333333333703, 0.3333333333333333703, 0.3333333333333333703, 0.3333333333333333703, 0.3333333333333333703, 0.3333333333333333703, 0.3333333333333333703, 0.3333333333333333703, 0.3333333333333333703, 0.3333333333333333703, 0.3333333333333333703, 0.3333333333333333703, 0.3333333333333333703, 0.3333333333333333703, 0.3333333333333333703, 0.3333333333333333703, 0.3333333333333333703, 0.3333333333333333703, 0.3333333333333333703, 0.3333333333333333703, 0.3333333333333333703, 0.3333333333333333703, 0.3333333333333333703, 0.3333333333333333703, 0.3333333333333333703, 0.3333333333333333703, 0.3333333333333333703, 0.3333333333333333703, 0.3333333333333333703, 0.3333333333333333703, 0.3333333333333333703, 0.3333333333333333703, 0.3333333333333333703, 0.3333333333333333703, 0.3333333333333333703, 0.3333333333333333703, 0.3333333333333333703, 0.3333333333333333703, 0.3333333333333333703, 0.3333333333333333703, 0.3333333333333333703, 0.3333333333333333703, 0.3333333333333333703, 0.3333333333333333703, 0.3333333333333333703, 0.3333333333333333703, 0.3333333333333333703, 0.3333333333333333703, 0.3333333333333333703, 0.3333333333333333703, 0.3333333333333333703, 0.3333333333333333703, 0.3333333333333333703, 0.3333333333333333703, 0.3333333333333333703, 0.3333333333333333703, 0.3333333333333333703, 0.3333333333333333703, 0.3333333333333333703, 0.3333333333333333703, 0.3333333333333333703, 0.3333333333333333703, 0.3333333333333333703, 0.3333333333333333703, 0.3333333333333333703, 0.3333333333333333703, 0.3333333333333333703, 0.3333333333333333703, 0.3333333333333333703, 0.3333333333333333703, 0.3333333333333333703, 0.3333333333333333703, 0.3333333333333333703, 0.3333333333333333703, 0.3333333333333333703, 0.3333333333333333703, 0.3333333333333333703, 0.3333333333333333703, 0.3333333333333333703, 0.3333333333333333703, 0.3333333333333333703, 0.3333333333333333703, 0.3333333333333333703, 0.3333333333333333703, 0.3333333333333333703, 0.3333333333333333703, 0.3333333333333333703, 0.3333333333333333703, 0.3333333333333333703, 0.3333333333333333703, 0.3333333333333333703, 0.3333333333333333703, 0.3333333333333333703, 0.3333333333333333703, 0.3333333333333333703, 0.3333333333333333703, 0.3333333333333333703, 0.3333333333333333703, 0.3333333333333333703, 0.3333333333333333703, 0.3333333333333333703, 0.3333333333333333703, 0.3333333333333333703, 0.3333333333333333703, 0.3333333333333333703, 0.3333333333333333703, 0.3333333333333333703, 0.3333333333333333703, 0.3333333333333333703, 0.3333333333333333703, 0.3333333333333333703, 0.3333333333333333703, 0.3333333333333333703, 0.3333333333333333703, 0.3333333333333333703),
 ( 1.000000000000000000, 1.000000000000000000, 1.000000000000000000, 1.000000000000000000, 1.000000000000000000, 1.000000000000000000, 1.000000000000000000, 1.000000000000000000, 1.000000000000000000, 1.000000000000000000, 1.000000000000000000, 1.000000000000000000, 1.000000000000000000, 1.000000000000000000, 1.000000000000000000, 1.000000000000000000, 1.000000000000000000, 1.000000000000000000, 1.000000000000000000, 1.000000000000000000, 1.000000000000000000, 1.000000000000000000, 1.000000000000000000, 1.000000000000000000, 1.000000000000000000, 1.000000000000000000, 1.000000000000000000, 1.000000000000000000, 1.000000000000000000, 1.000000000000000000, 1.000000000000000000, 1.000000000000000000, 1.000000000000000000, 1.000000000000000000, 1.000000000000000000, 1.000000000000000000, 1.000000000000000000, 1.000000000000000000, 1.000000000000000000, 1.000000000000000000, 1.000000000000000000, 1.000000000000000000, 1.000000000000000000, 1.000000000000000000, 1.000000000000000000, 1.000000000000000000, 1.000000000000000000, 1.000000000000000000, 1.000000000000000000, 1.000000000000000000, 1.000000000000000000, 1.000000000000000000, 1.000000000000000000, 1.000000000000000000, 1.000000000000000000, 1.000000000000000000, 1.000000000000000000, 1.000000000000000000, 1.000000000000000000, 1.000000000000000000, 1.000000000000000000, 1.000000000000000000, 1.000000000000000000, 1.000000000000000000, 1.000000000000000000, 1.000000000000000000, 1.000000000000000000, 1.000000000000000000, 1.000000000000000000, 1.000000000000000000, 1.000000000000000000, 1.000000000000000000, 1.000000000000000000, 1.000000000000000000, 1.000000000000000000, 1.000000000000000000, 1.000000000000000000, 1.000000000000000000, 1.000000000000000000, 1.000000000000000000, 1.000000000000000000, 1.000000000000000000, 1.000000000000000000, 1.000000000000000000, 1.000000000000000000, 1.000000000000000000, 1.000000000000000000, 1.000000000000000000, 1.000000000000000000, 1.000000000000000000, 1.000000000000000000, 1.000000000000000000, 1.000000000000000000, 1.000000000000000000, 1.000000000000000000, 1.000000000000000000, 1.000000000000000000, 1.000000000000000000, 1.000000000000000000, 1.000000000000000000, 1.000000000000000000, 1.000000000000000000, 1.000000000000000000, 1.000000000000000000, 1.000000000000000000, 1.000000000000000000, 1.000000000000000000, 1.000000000000000000, 1.000000000000000000, 1.000000000000000000, 1.000000000000000000, 1.000000000000000000, 1.000000000000000000, 1.000000000000000000, 1.000000000000000000, 1.000000000000000000, 1.000000000000000000, 1.000000000000000000, 1.000000000000000000, 1.000000000000000000, 1.000000000000000000, 1.000000000000000000, 1.000000000000000000, 1.000000000000000000, 1.000000000000000000, 1.000000000000000000, 1.000000000000000000, 1.000000000000000000, 1.000000000000000000, 1.000000000000000000, 1.000000000000000000, 1.000000000000000000, 1.000000000000000000, 1.000000000000000000, 1.000000000000000000, 1.000000000000000000, 1.000000000000000000, 1.000000000000000000, 1.000000000000000000, 1.000000000000000000, 1.000000000000000000, 1.000000000000000000, 1.000000000000000000, 1.000000000000000000, 1.000000000000000000, 1.000000000000000000, 1.000000000000000000, 1.000000000000000000, 1.000000000000000000, 1.000000000000000000, 1.000000000000000000, 1.000000000000000000, 1.000000000000000000, 1.000000000000000000, 1.000000000000000000, 1.000000000000000000, 1.000000000000000000, 1.000000000000000000, 1.000000000000000000, 1.000000000000000000, 1.000000000000000000, 1.000000000000000000),
 ( 0.3333333333333333703, 0.3333333333333333703, 0.3333333333333333703, 0.3333333333333333703, 0.3333333333333333703, 0.3333333333333333703, 0.3333333333333333703, 0.3333333333333333703, 0.3333333333333333703, 0.3333333333333333703, 0.3333333333333333703, 0.3333333333333333703, 0.3333333333333333703, 0.3333333333333333703, 0.3333333333333333703, 0.3333333333333333703, 0.3333333333333333703, 0.3333333333333333703, 0.3333333333333333703, 0.3333333333333333703, 0.3333333333333333703, 0.3333333333333333703, 0.3333333333333333703, 0.3333333333333333703, 0.3333333333333333703, 0.3333333333333333703, 0.3333333333333333703, 0.3333333333333333703, 0.3333333333333333703, 0.3333333333333333703, 0.3333333333333333703, 0.3333333333333333703, 0.3333333333333333703, 0.3333333333333333703, 0.3333333333333333703, 0.3333333333333333703, 0.3333333333333333703, 0.3333333333333333703, 0.3333333333333333703, 0.3333333333333333703, 0.3333333333333333703, 0.3333333333333333703, 0.3333333333333333703, 0.3333333333333333703, 0.3333333333333333703, 0.3333333333333333703, 0.3333333333333333703, 0.3333333333333333703, 0.3333333333333333703, 0.3333333333333333703, 0.3333333333333333703, 0.3333333333333333703, 0.3333333333333333703, 0.3333333333333333703, 0.3333333333333333703, 0.3333333333333333703, 0.3333333333333333703, 0.3333333333333333703, 0.3333333333333333703, 0.3333333333333333703, 0.3333333333333333703, 0.3333333333333333703, 0.3333333333333333703, 0.3333333333333333703, 0.3333333333333333703, 0.3333333333333333703, 0.3333333333333333703, 0.3333333333333333703, 0.3333333333333333703, 0.3333333333333333703, 0.3333333333333333703, 0.3333333333333333703, 0.3333333333333333703, 0.3333333333333333703, 0.3333333333333333703, 0.3333333333333333703, 0.3333333333333333703, 0.3333333333333333703, 0.3333333333333333703, 0.3333333333333333703, 0.3333333333333333703, 0.3333333333333333703, 0.3333333333333333703, 0.3333333333333333703, 0.3333333333333333703, 0.3333333333333333703, 0.3333333333333333703, 0.3333333333333333703, 0.3333333333333333703, 0.3333333333333333703, 0.3333333333333333703, 0.3333333333333333703, 0.3333333333333333703, 0.3333333333333333703, 0.3333333333333333703, 0.3333333333333333703, 0.3333333333333333703, 0.3333333333333333703, 0.3333333333333333703, 0.3333333333333333703, 0.3333333333333333703, 0.3333333333333333703, 0.3333333333333333703, 0.3333333333333333703, 0.3333333333333333703, 0.3333333333333333703, 0.3333333333333333703, 0.3333333333333333703, 0.3333333333333333703, 0.3333333333333333703, 0.3333333333333333703, 0.3333333333333333703, 0.3333333333333333703, 0.3333333333333333703, 0.3333333333333333703, 0.3333333333333333703, 0.3333333333333333703, 0.3333333333333333703, 0.3333333333333333703, 0.3333333333333333703, 0.3333333333333333703, 0.3333333333333333703, 0.3333333333333333703, 0.3333333333333333703, 0.3333333333333333703, 0.3333333333333333703, 0.3333333333333333703, 0.3333333333333333703, 0.3333333333333333703, 0.3333333333333333703, 0.3333333333333333703, 0.3333333333333333703, 0.3333333333333333703, 0.3333333333333333703, 0.3333333333333333703, 0.3333333333333333703, 0.3333333333333333703, 0.3333333333333333703, 0.3333333333333333703, 0.3333333333333333703, 0.3333333333333333703, 0.3333333333333333703, 0.3333333333333333703, 0.3333333333333333703, 0.3333333333333333703, 0.3333333333333333703, 0.3333333333333333703, 0.3333333333333333703, 0.3333333333333333703, 0.3333333333333333703, 0.3333333333333333703, 0.3333333333333333703, 0.3333333333333333703, 0.3333333333333333703, 0.3333333333333333703, 0.3333333333333333703, 0.3333333333333333703, 0.3333333333333333703, 0.3333333333333333703, 0.3333333333333333703, 0.3333333333333333703, 0.3333333333333333703),
 ( 0.3333333333333333703, 0.3333333333333333703, 0.3333333333333333703, 0.3333333333333333703, 0.3333333333333333703, 0.3333333333333333703, 0.3333333333333333703, 0.3333333333333333703, 0.3333333333333333703, 0.3333333333333333703, 0.3333333333333333703, 0.3333333333333333703, 0.3333333333333333703, 0.3333333333333333703, 0.3333333333333333703, 0.3333333333333333703, 0.3333333333333333703, 0.3333333333333333703, 0.3333333333333333703, 0.3333333333333333703, 0.3333333333333333703, 0.3333333333333333703, 0.3333333333333333703, 0.3333333333333333703, 0.3333333333333333703, 0.3333333333333333703, 0.3333333333333333703, 0.3333333333333333703, 0.3333333333333333703, 0.3333333333333333703, 0.3333333333333333703, 0.3333333333333333703, 0.3333333333333333703, 0.3333333333333333703, 0.3333333333333333703, 0.3333333333333333703, 0.3333333333333333703, 0.3333333333333333703, 0.3333333333333333703, 0.3333333333333333703, 0.3333333333333333703, 0.3333333333333333703, 0.3333333333333333703, 0.3333333333333333703, 0.3333333333333333703, 0.3333333333333333703, 0.3333333333333333703, 0.3333333333333333703, 0.3333333333333333703, 0.3333333333333333703, 0.3333333333333333703, 0.3333333333333333703, 0.3333333333333333703, 0.3333333333333333703, 0.3333333333333333703, 0.3333333333333333703, 0.3333333333333333703, 0.3333333333333333703, 0.3333333333333333703, 0.3333333333333333703, 0.3333333333333333703, 0.3333333333333333703, 0.3333333333333333703, 0.3333333333333333703, 0.3333333333333333703, 0.3333333333333333703, 0.3333333333333333703, 0.3333333333333333703, 0.3333333333333333703, 0.3333333333333333703, 0.3333333333333333703, 0.3333333333333333703, 0.3333333333333333703, 0.3333333333333333703, 0.3333333333333333703, 0.3333333333333333703, 0.3333333333333333703, 0.3333333333333333703, 0.3333333333333333703, 0.3333333333333333703, 0.3333333333333333703, 0.3333333333333333703, 0.3333333333333333703, 0.3333333333333333703, 0.3333333333333333703, 0.3333333333333333703, 0.3333333333333333703, 0.3333333333333333703, 0.3333333333333333703, 0.3333333333333333703, 0.3333333333333333703, 0.3333333333333333703, 0.3333333333333333703, 0.3333333333333333703, 0.3333333333333333703, 0.3333333333333333703, 0.3333333333333333703, 0.3333333333333333703, 0.3333333333333333703, 0.3333333333333333703, 0.3333333333333333703, 0.3333333333333333703, 0.3333333333333333703, 0.3333333333333333703, 0.3333333333333333703, 0.3333333333333333703, 0.3333333333333333703, 0.3333333333333333703, 0.3333333333333333703, 0.3333333333333333703, 0.3333333333333333703, 0.3333333333333333703, 0.3333333333333333703, 0.3333333333333333703, 0.3333333333333333703, 0.3333333333333333703, 0.3333333333333333703, 0.3333333333333333703, 0.3333333333333333703, 0.3333333333333333703, 0.3333333333333333703, 0.3333333333333333703, 0.3333333333333333703, 0.3333333333333333703, 0.3333333333333333703, 0.3333333333333333703, 0.3333333333333333703, 0.3333333333333333703, 0.3333333333333333703, 0.3333333333333333703, 0.3333333333333333703, 0.3333333333333333703, 0.3333333333333333703, 0.3333333333333333703, 0.3333333333333333703, 0.3333333333333333703, 0.3333333333333333703, 0.3333333333333333703, 0.3333333333333333703, 0.3333333333333333703, 0.3333333333333333703, 0.3333333333333333703, 0.3333333333333333703, 0.3333333333333333703, 0.3333333333333333703, 0.3333333333333333703, 0.3333333333333333703, 0.3333333333333333703, 0.3333333333333333703, 0.3333333333333333703, 0.3333333333333333703, 0.3333333333333333703, 0.3333333333333333703, 0.3333333333333333703, 0.3333333333333333703, 0.3333333333333333703, 0.3333333333333333703, 0.3333333333333333703, 0.3333333333333333703, 0.3333333333333333703, 0.3333333333333333703, 0.3333333333333333703),
 ( 1.000000000000000000, 1.000000000000000000, 1.000000000000000000, 1.000000000000000000, 1.000000000000000000, 1.000000000000000000, 1.000000000000000000, 1.000000000000000000, 1.000000000000000000, 1.000000000000000000, 1.000000000000000000, 1.000000000000000000, 1.000000000000000000, 1.000000000000000000, 1.000000000000000000, 1.000000000000000000, 1.000000000000000000, 1.000000000000000000, 1.000000000000000000, 1.000000000000000000, 1.000000000000000000, 1.000000000000000000, 1.000000000000000000, 1.000000000000000000, 1.000000000000000000, 1.000000000000000000, 1.000000000000000000, 1.000000000000000000, 1.000000000000000000, 1.000000000000000000, 1.000000000000000000, 1.000000000000000000, 1.000000000000000000, 1.000000000000000000, 1.000000000000000000, 1.000000000000000000, 1.000000000000000000, 1.000000000000000000, 1.000000000000000000, 1.000000000000000000, 1.000000000000000000, 1.000000000000000000, 1.000000000000000000, 1.000000000000000000, 1.000000000000000000, 1.000000000000000000, 1.000000000000000000, 1.000000000000000000, 1.000000000000000000, 1.000000000000000000, 1.000000000000000000, 1.000000000000000000, 1.000000000000000000, 1.000000000000000000, 1.000000000000000000, 1.000000000000000000, 1.000000000000000000, 1.000000000000000000, 1.000000000000000000, 1.000000000000000000, 1.000000000000000000, 1.000000000000000000, 1.000000000000000000, 1.000000000000000000, 1.000000000000000000, 1.000000000000000000, 1.000000000000000000, 1.000000000000000000, 1.000000000000000000, 1.000000000000000000, 1.000000000000000000, 1.000000000000000000, 1.000000000000000000, 1.000000000000000000, 1.000000000000000000, 1.000000000000000000, 1.000000000000000000, 1.000000000000000000, 1.000000000000000000, 1.000000000000000000, 1.000000000000000000, 1.000000000000000000, 1.000000000000000000, 1.000000000000000000, 1.000000000000000000, 1.000000000000000000, 1.000000000000000000, 1.000000000000000000, 1.000000000000000000, 1.000000000000000000, 1.000000000000000000, 1.000000000000000000, 1.000000000000000000, 1.000000000000000000, 1.000000000000000000, 1.000000000000000000, 1.000000000000000000, 1.000000000000000000, 1.000000000000000000, 1.000000000000000000, 1.000000000000000000, 1.000000000000000000, 1.000000000000000000, 1.000000000000000000, 1.000000000000000000, 1.000000000000000000, 1.000000000000000000, 1.000000000000000000, 1.000000000000000000, 1.000000000000000000, 1.000000000000000000, 1.000000000000000000, 1.000000000000000000, 1.000000000000000000, 1.000000000000000000, 1.000000000000000000, 1.000000000000000000, 1.000000000000000000, 1.000000000000000000, 1.000000000000000000, 1.000000000000000000, 1.000000000000000000, 1.000000000000000000, 1.000000000000000000, 1.000000000000000000, 1.000000000000000000, 1.000000000000000000, 1.000000000000000000, 1.000000000000000000, 1.000000000000000000, 1.000000000000000000, 1.000000000000000000, 1.000000000000000000, 1.000000000000000000, 1.000000000000000000, 1.000000000000000000, 1.000000000000000000, 1.000000000000000000, 1.000000000000000000, 1.000000000000000000, 1.000000000000000000, 1.000000000000000000, 1.000000000000000000, 1.000000000000000000, 1.000000000000000000, 1.000000000000000000, 1.000000000000000000, 1.000000000000000000, 1.000000000000000000, 1.000000000000000000, 1.000000000000000000, 1.000000000000000000, 1.000000000000000000, 1.000000000000000000, 1.000000000000000000, 1.000000000000000000, 1.000000000000000000, 1.000000000000000000, 1.000000000000000000, 1.000000000000000000, 1.000000000000000000, 1.000000000000000000) ) ) 
 REPRESENTATION_ITEM ( '' )  SURFACE ( )  );
#13706 = CARTESIAN_POINT ( 'NONE',  ( 47.05648932407426344, 100.9104996726487400, 37.14960608071593384 ) ) ;
#13707 = CARTESIAN_POINT ( 'NONE',  ( 136.2768881589198884, 181.8432453435730167, 21.73429951086134082 ) ) ;
#13708 = CARTESIAN_POINT ( 'NONE',  ( 89.42064422693164261, 282.0082918409407284, -4.000000000000004441 ) ) ;
#13709 = CARTESIAN_POINT ( 'NONE',  ( 47.43856463449118621, 97.87977050742732388, 34.21067981925357060 ) ) ;
#13710 = CARTESIAN_POINT ( 'NONE',  ( 26.65597624659334031, 142.8797025615743337, -3.772066457372480475 ) ) ;
#13711 = CARTESIAN_POINT ( 'NONE',  ( -157.2955611005346270, -169.4438272943107222, 57.67623309621198047 ) ) ;
#13712 = CARTESIAN_POINT ( 'NONE',  ( 47.43856463449118621, 79.61518717409400381, 34.21067981925357060 ) ) ;
#13713 = CARTESIAN_POINT ( 'NONE',  ( -138.5468111011521160, 759.4679229819337252, -23.16745088979876499 ) ) ;
#13714 = DIRECTION ( 'NONE',  ( 0.000000000000000000, 1.000000000000000000, 0.000000000000000000 ) ) ;
#13715 = VERTEX_POINT ( 'NONE', #21188 ) ;
#13716 = CARTESIAN_POINT ( 'NONE',  ( -151.4692556286852891, -176.3130981290892976, 39.65701158161629536 ) ) ;
#13717 = CARTESIAN_POINT ( 'NONE',  ( -156.1828648351502409, -155.3945647575688156, 41.49286807254280518 ) ) ;
#13718 = CARTESIAN_POINT ( 'NONE',  ( 40.27526882409969744, 141.8297705074273267, 37.97664729208901235 ) ) ;
#13719 = CARTESIAN_POINT ( 'NONE',  ( 59.14563986918259531, 96.87627350248034475, 7.732070471200789719 ) ) ;
#13720 = VERTEX_POINT ( 'NONE', #11361 ) ;
#13721 = CARTESIAN_POINT ( 'NONE',  ( 54.85617982533818804, 239.2521282348021714, -3.999999999999980904 ) ) ;
#13722 = VERTEX_POINT ( 'NONE', #16104 ) ;
#13723 = CARTESIAN_POINT ( 'NONE',  ( 45.74753988029933538, 134.3297705074273267, 30.44471234641811819 ) ) ;
#13724 = B_SPLINE_CURVE_WITH_KNOTS ( 'NONE', 3,
 ( #11713, #15020, #13484, #6013, #18448, #11492, #15134, #3346, #10074, #14498, #4886, #16783, #6543, #16557, #13268, #4355, #14391, #12743, #3125, #7794, #1694, #6668, #1472, #19465, #20216, #9855, #1583, #11084, #20002, #1062, #8425, #18219, #19883, #5109, #17798, #16671, #17694, #2596, #18335, #4771, #9335, #16035, #949, #2709, #8204, #16152, #21241, #6119, #13153, #14905, #21654, #11607, #3236, #9968, #15666, #15248, #7200, #569, #1803, #15564, #10509, #14014, #20321, #17318, #11933, #467, #18664, #2228, #18770, #20642, #5525, #17101, #10612, #146, #18558, #8536, #7313, #12139, #6989, #15465, #13903, #6877, #2121, #13693, #3671, #20747, #10401, #3780, #13584, #12254, #3463, #11825, #10187, #5220, #17205, #18985, #16889, #3889, #8959, #16994, #3568, #10292, #20427, #1903, #8638, #8857, #15360, #12039, #251, #2017, #20536, #5323, #8748, #366, #7093, #13798, #5422, #18873, #17811, #9463, #2722, #15945, #19475, #6024, #5806, #10994, #14511, #16163, #20924, #855, #1075, #7376, #5705, #11098, #19266, #12537, #14291, #21252, #9137, #12429, #10677, #7805, #6132, #4266, #4166, #961, #19155, #17704, #4056, #10895, #17598, #5919, #10784, #17491, #2401, #12861, #2504, #15837, #3951, #7592, #2286, #21140 ),
 .UNSPECIFIED., .F., .F.,
 ( 4, 2, 2, 2, 2, 2, 2, 2, 2, 2, 2, 2, 2, 2, 2, 2, 2, 2, 2, 2, 2, 2, 2, 2, 2, 2, 2, 2, 2, 2, 2, 2, 2, 2, 2, 2, 2, 2, 2, 2, 2, 2, 2, 2, 2, 2, 2, 2, 2, 2, 2, 2, 2, 2, 2, 2, 2, 2, 2, 2, 2, 2, 2, 2, 2, 2, 2, 2, 2, 2, 2, 2, 2, 2, 2, 2, 2, 2, 2, 2, 4 ),
 ( 0.000000000000000000, 0.008318061648474830982, 0.01871563870907547167, 0.02911321576967611582, 0.03951079283027675998, 0.04990836989087740067, 0.06030594695147804829, 0.07070352401207868898, 0.08110110107267932966, 0.09149867813327997035, 0.1018962551938806110, 0.1122938322544812378, 0.1226914093150818785, 0.1330889863756825053, 0.1434865634362831321, 0.1538841404968837590, 0.1642817175574844135, 0.1746792946180850126, 0.1850768716786856394, 0.1954744487392862939, 0.2058720257998869485, 0.2162696028604875753, 0.2266671799210882021, 0.2370647569816888289, 0.2474623340422894557, 0.2578599111028900825, 0.2682574881634907094, 0.2786550652240913362, 0.2890526422846919630, 0.2994502193452925343, 0.3098477964058931611, 0.3202453734664938434, 0.3306429505270944147, 0.3410405275876950415, 0.3514381046482956683, 0.3618356817088962951, 0.3722332587694969219, 0.3826308358300975487, 0.3930284128906983421, 0.4034259899512990799, 0.4138235670118998732, 0.4242211440725006666, 0.4346187211331003497, 0.4450162981936999218, 0.4554138752542995494, 0.4658114523148991770, 0.4762090293755007475, 0.4866066064361022070, 0.4970041834967036110, 0.5074017605573051259, 0.5177993376179057528, 0.5281969146785063796, 0.5385944917391070064, 0.5489920687997077442, 0.5593896458603083710, 0.5697872229209089978, 0.5801847999815096246, 0.5905823770421102514, 0.6009799541027108782, 0.6113775311633115050, 0.6217751082239121319, 0.6321726852845127587, 0.6425702623451133855, 0.6529678394057140123, 0.6633654164663146391, 0.6737629935269153769, 0.6841605705875142274, 0.6945581476481129668, 0.7049557247087120393, 0.7153533017693110008, 0.7257508788299132929, 0.7361484558905155851, 0.7465460329511179882, 0.7569436100117202804, 0.7673411870723210182, 0.7777387641329215340, 0.7881363411935222718, 0.7985339182541228986, 0.8080132075800156022, 0.8174924969059083057, 0.8280181261579530050 ),
 .UNSPECIFIED. ) ;
#13725 = EDGE_CURVE ( 'NONE', #470, #12132, #2988, .T. ) ;
#13726 = CARTESIAN_POINT ( 'NONE',  ( 44.37947211624943833, 61.01518717409400239, 38.42115945441014446 ) ) ;
#13727 = LINE ( 'NONE', #7130, #15550 ) ;
#13728 = LINE ( 'NONE', #16401, #4560 ) ;
#13729 = CARTESIAN_POINT ( 'NONE',  ( -142.0420953463935803, -156.5438272943107449, 52.72008163687743831 ) ) ;
#13730 = PLANE ( 'NONE',  #5801 ) ;
#13731 = CARTESIAN_POINT ( 'NONE',  ( -143.3790856849358306, -171.3630981290893089, 55.53486410454105027 ) ) ;
#13732 = CARTESIAN_POINT ( 'NONE',  ( -22.33874983538537506, 60.77209968883889957, 1.734723475976807094E-15 ) ) ;
#13733 = CARTESIAN_POINT ( 'NONE',  ( 41.46631938032478359, 138.3844580088725991, 38.96596240072933170 ) ) ;
#13734 = CARTESIAN_POINT ( 'NONE',  ( 41.64333658814960870, 126.9797705074273182, 38.42115945441014446 ) ) ;
#13735 = CARTESIAN_POINT ( 'NONE',  ( 20.05807715703862470, 136.4285572017038248, 1.866423417236719118 ) ) ;
#13736 = CARTESIAN_POINT ( 'NONE',  ( 147.5268905834513475, 193.0332408774651185, 272.0939500981630204 ) ) ;
#13737 = CARTESIAN_POINT ( 'NONE',  ( 39.42975644700377558, 110.8151871740939924, 31.60846029578754468 ) ) ;
#13738 = EDGE_CURVE ( 'NONE', #255, #2224, #17970, .T. ) ;
#13739 = FACE_OUTER_BOUND ( 'NONE', #11686, .T. ) ;
#13740 = CARTESIAN_POINT ( 'NONE',  ( 11.23391594879739941, 132.3357020601377769, 10.49983985543964415 ) ) ;
#13741 = CARTESIAN_POINT ( 'NONE',  ( 37.56771007382699423, 92.23784766911828115, 0.6328166970475824771 ) ) ;
#13742 = ADVANCED_BREP_SHAPE_REPRESENTATION ( '', ( #14370, #12657 ), #343 ) ;
#13743 = CARTESIAN_POINT ( 'NONE',  ( 173.3794444120442506, -84.13255853780189852, 5.000000000000018652 ) ) ;
#13744 = CARTESIAN_POINT ( 'NONE',  ( 38.58424406990785371, 87.52977050742730114, 35.64915139335015937 ) ) ;
#13745 = VERTEX_POINT ( 'NONE', #1014 ) ;
#13746 = CARTESIAN_POINT ( 'NONE',  ( 44.55648932407425633, 133.6104996726487286, 38.96596240072933170 ) ) ;
#13747 = CARTESIAN_POINT ( 'NONE',  ( 41.46631938032478359, 74.18445800887258201, 29.45539723777780239 ) ) ;
#13748 = CARTESIAN_POINT ( 'NONE',  ( 38.01140435219952707, 86.93445800887258201, 35.83527830041809636 ) ) ;
#13749 = CARTESIAN_POINT ( 'NONE',  ( 47.05648932407426344, 125.5104996726487343, 31.27175355779120025 ) ) ;
#13750 = CARTESIAN_POINT ( 'NONE',  ( 44.37947211624943833, 83.21518717409399812, 30.00020018409699318 ) ) ;
#13751 = ADVANCED_FACE ( 'NONE', ( #3103 ), #1228, .T. ) ;
#13752 = CARTESIAN_POINT ( 'NONE',  ( -148.3790856849358306, -195.3891397928654783, 40.14644641866477315 ) ) ;
#13753 = CARTESIAN_POINT ( 'NONE',  ( -157.2955611005345986, -176.3438272943106995, 41.63779006702063867 ) ) ;
#13754 = CARTESIAN_POINT ( 'NONE',  ( -145.2889157411863437, -177.5391397928654840, 41.15050349809589392 ) ) ;
#13755 = CARTESIAN_POINT ( 'NONE',  ( -157.6495955161842062, -193.1130981290893374, 58.16351966513671812 ) ) ;
#13756 = FACE_OUTER_BOUND ( 'NONE', #9908, .T. ) ;
#13757 = CARTESIAN_POINT ( 'NONE',  ( 38.96631938032478359, 92.48445800887257917, 31.27175355779120025 ) ) ;
#13758 = LINE ( 'NONE', #3957, #11140 ) ;
#13759 = CARTESIAN_POINT ( 'NONE',  ( 47.43856463449117200, 154.7297705074273040, 35.64915139335016647 ) ) ;
#13760 = CARTESIAN_POINT ( 'NONE',  ( 40.27526882409969033, 102.8297705074272983, 37.97664729208901946 ) ) ;
#13761 = CARTESIAN_POINT ( 'NONE',  ( 60.35187701982888342, 149.5179833730722407, -3.570052342179399485 ) ) ;
#13762 = CARTESIAN_POINT ( 'NONE',  ( 45.74753988029934249, 140.0651871740940067, 30.44471234641812174 ) ) ;
#13763 = CARTESIAN_POINT ( 'NONE',  ( -151.4692556286852891, -163.4084106276440309, 59.56931450028537256 ) ) ;
#13764 = CARTESIAN_POINT ( 'NONE',  ( 147.5268905834513475, 193.0332408774651185, -19.99999999999997868 ) ) ;
#13765 =( BOUNDED_CURVE ( )  B_SPLINE_CURVE ( 2, ( #2260, #8997, #15705, #611, #7347, #14051, #4341 ),
 .UNSPECIFIED., .F., .F. ) 
 B_SPLINE_CURVE_WITH_KNOTS ( ( 3, 2, 2, 3 ),
 ( 0.000000000000000000, 0.007142857142857142634, 0.01428571428571428527, 0.01785714285714287350 ),
 .UNSPECIFIED. ) 
 CURVE ( )  GEOMETRIC_REPRESENTATION_ITEM ( )  RATIONAL_B_SPLINE_CURVE ( ( 1.000000000000000000, 0.9510565162951535312, 1.000000000000000000, 0.9510565162951535312, 1.000000000000000000, 0.9755282581475765991, 0.9755282581475767101 ) ) 
 REPRESENTATION_ITEM ( '' )  );
#13766 = CARTESIAN_POINT ( 'NONE',  ( 59.79647059797250819, 142.6686746773435459, -3.371582063846674693 ) ) ;
#13767 = CARTESIAN_POINT ( 'NONE',  ( 43.01140435219951286, 119.3651871740939896, 29.55568802177586463 ) ) ;
#13768 = EDGE_CURVE ( 'NONE', #18531, #8368, #6408, .T. ) ;
#13769 = ORIENTED_EDGE ( 'NONE', *, *, #18244, .F. ) ;
#13770 = EDGE_LOOP ( 'NONE', ( #9386, #5499, #6373, #287 ) ) ;
#13771 = LINE ( 'NONE', #5610, #5012 ) ;
#13772 = VERTEX_POINT ( 'NONE', #14778 ) ;
#13773 = EDGE_CURVE ( 'NONE', #5574, #2417, #4416, .T. ) ;
#13774 = CARTESIAN_POINT ( 'NONE',  ( 48.01140435219951996, 97.28445800887259054, 34.21067981925357060 ) ) ;
#13775 = PRODUCT_DEFINITION_SHAPE ( 'NONE', 'NONE',  #16589 ) ;
#13776 = CARTESIAN_POINT ( 'NONE',  ( 38.01140435219951996, 156.8604996726487855, 35.83527830041810347 ) ) ;
#13778 = CARTESIAN_POINT ( 'NONE',  ( 52.77336176550079472, 93.53620953014643646, -12.98192714454240182 ) ) ;
#13777 = CARTESIAN_POINT ( 'NONE',  ( 38.58424406990784661, 117.2651871740940095, 35.64915139335016647 ) ) ;
#13779 = CARTESIAN_POINT ( 'NONE',  ( 46.10157429594899270, 70.76049967264873430, 38.46393386101376421 ) ) ;
#13781 = CARTESIAN_POINT ( 'NONE',  ( 38.96631938032478359, 74.48445800887257917, 31.27175355779120025 ) ) ;
#13780 = FACE_OUTER_BOUND ( 'NONE', #14989, .T. ) ;
#13782 = CARTESIAN_POINT ( 'NONE',  ( 111.4021762516569964, 137.5714195593754710, -19.99999999999997868 ) ) ;
#13783 = CARTESIAN_POINT ( 'NONE',  ( 45.52178281274064631, 95.03194855707397437, 29.87433574750618703 ) ) ;
#13784 = CARTESIAN_POINT ( 'NONE',  ( 44.37947211624943833, 77.21518717409399812, 30.00020018409699318 ) ) ;
#13785 = CARTESIAN_POINT ( 'NONE',  ( 175.9120630731088397, 202.0864028065961122, 21.73429951086134082 ) ) ;
#13786 = CARTESIAN_POINT ( 'NONE',  ( -145.6429501568359797, -177.8438272943106995, 57.67623309621198047 ) ) ;
#13787 = DIRECTION ( 'NONE',  ( 0.000000000000000000, 0.000000000000000000, 1.000000000000000000 ) ) ;
#13788 = EDGE_LOOP ( 'NONE', ( #3672, #17546, #7258, #13131, #21125, #13879, #4128, #15935 ) ) ;
#13789 = CARTESIAN_POINT ( 'NONE',  ( -160.8964159109769696, -188.1584106276440593, 49.65701158161630957 ) ) ;
#13790 = CARTESIAN_POINT ( 'NONE',  ( 8.829984022807513711, 121.7968051057545580, 16.14860047415989541 ) ) ;
#13791 = CARTESIAN_POINT ( 'NONE',  ( -157.2955611005346270, -179.6084106276440764, 41.63779006702063867 ) ) ;
#13792 = ORIENTED_EDGE ( 'NONE', *, *, #20803, .F. ) ;
#13793 = VECTOR ( 'NONE', #8082, 1000.000000000000000 ) ;
#13794 = CARTESIAN_POINT ( 'NONE',  ( 38.58424406990784661, 140.9651871740939555, 32.77220824515698183 ) ) ;
#13795 = AXIS2_PLACEMENT_3D ( 'NONE', #7280, #7496, #14197 ) ;
#13796 = CARTESIAN_POINT ( 'NONE',  ( 47.43856463449117911, 157.7651871740940237, 32.77220824515697473 ) ) ;
#13797 = CARTESIAN_POINT ( 'NONE',  ( 47.43856463449118621, 106.8797705074273239, 34.21067981925357060 ) ) ;
#13798 = CARTESIAN_POINT ( 'NONE',  ( 9.822352152143091431, 128.2981216602131553, 9.363167623699879982 ) ) ;
#13799 = EDGE_LOOP ( 'NONE', ( #8744, #18422, #6115, #1586, #20797, #5767 ) ) ;
#13800 = AXIS2_PLACEMENT_3D ( 'NONE', #13785, #20524, #15768 ) ;
#13801 = CARTESIAN_POINT ( 'NONE',  ( 65.09246388851926213, 137.4469437283422906, 4.918530982704383270 ) ) ;
#13802 = VERTEX_POINT ( 'NONE', #6522 ) ;
#13803 = LINE ( 'NONE', #12144, #20056 ) ;
#13804 = CARTESIAN_POINT ( 'NONE',  ( 38.01140435219952707, 128.6344580088725706, 32.58608133808903773 ) ) ;
#13805 = SHAPE_REPRESENTATION ( 'Lower Fixed Base Shear Blade', ( #12657 ), #343 ) ;
#13806 = CARTESIAN_POINT ( 'NONE',  ( 45.74753988029933538, 83.32977050742732672, 30.44471234641811819 ) ) ;
#13807 = CARTESIAN_POINT ( 'NONE',  ( 45.74753988029933538, 143.0651871740939782, 30.44471234641811819 ) ) ;
#13808 = CARTESIAN_POINT ( 'NONE',  ( 44.55648932407425633, 101.8104996726487457, 29.45539723777780239 ) ) ;
#13809 = CARTESIAN_POINT ( 'NONE',  ( 13.78455932396994577, 137.7305411390292420, 2.696406107442721467 ) ) ;
#13810 = CARTESIAN_POINT ( 'NONE',  ( -151.4692556286853176, -175.7391397928654726, 59.65701158161632378 ) ) ;
#13811 = CARTESIAN_POINT ( 'NONE',  ( -161.4692556286853176, -173.4891397928654726, 49.65701158161630957 ) ) ;
#13812 = DIRECTION ( 'NONE',  ( -0.000000000000000000, 1.000000000000000000, -0.000000000000000000 ) ) ;
#13813 = DIRECTION ( 'NONE',  ( 0.000000000000000000, 0.000000000000000000, 1.000000000000000000 ) ) ;
#13814 = CARTESIAN_POINT ( 'NONE',  ( 44.55648932407425633, 91.61049967264874283, 38.96596240072933170 ) ) ;
#13815 = CARTESIAN_POINT ( 'NONE',  ( 46.59305225739526435, 88.57977050742732672, 36.81289934271958941 ) ) ;
#13816 = CARTESIAN_POINT ( 'NONE',  ( 69.04633063039527485, 130.7408809369782716, -8.772150750671475095 ) ) ;
#13817 = CARTESIAN_POINT ( 'NONE',  ( -148.5561028927606344, -173.7938272943107165, 40.69124936498395328 ) ) ;
#13818 = CARTESIAN_POINT ( 'NONE',  ( 43.01140435219951286, 74.36518717409400381, 29.55568802177586107 ) ) ;
#13819 = CARTESIAN_POINT ( 'NONE',  ( -161.4692556286852891, -170.6391397928654499, 46.40781461928724383 ) ) ;
#13820 = DIRECTION ( 'NONE',  ( -0.9385982292947087080, -0.3450121214752278620, 1.836742322155470738E-16 ) ) ;
#13821 = ORIENTED_EDGE ( 'NONE', *, *, #9831, .F. ) ;
#13822 = EDGE_CURVE ( 'NONE', #1116, #12681, #17753, .T. ) ;
#13823 = EDGE_CURVE ( 'NONE', #9846, #10182, #920, .T. ) ;
#13824 = CARTESIAN_POINT ( 'NONE',  ( 47.05648932407426344, 84.98445800887257917, 37.14960608071593384 ) ) ;
#13825 = LINE ( 'NONE', #2042, #14135 ) ;
#13826 = CARTESIAN_POINT ( 'NONE',  ( 40.27526882409969744, 132.8297705074272983, 37.97664729208901235 ) ) ;
#13827 = CARTESIAN_POINT ( 'NONE',  ( 23.25700774553339301, 99.89415360575743819, 9.279811863844059872 ) ) ;
#13828 = ORIENTED_EDGE ( 'NONE', *, *, #1272, .F. ) ;
#13829 = CYLINDRICAL_SURFACE ( 'NONE', #15706, 7.500000000000007105 ) ;
#13830 = ORIENTED_EDGE ( 'NONE', *, *, #12584, .F. ) ;
#13831 = CARTESIAN_POINT ( 'NONE',  ( 38.58424406990784661, 132.5297705074272869, 35.64915139335016647 ) ) ;
#13832 = CARTESIAN_POINT ( 'NONE',  ( 46.59305225739526435, 91.57977050742731251, 36.81289934271958941 ) ) ;
#13833 =( BOUNDED_CURVE ( )  B_SPLINE_CURVE ( 2, ( #21036, #17381, #14077, #15737, #642, #20815, #9347, #12647, #19369, #14403, #16051, #7704, #748 ),
 .UNSPECIFIED., .F., .T. ) 
 B_SPLINE_CURVE_WITH_KNOTS ( ( 3, 2, 2, 2, 2, 2, 3 ),
 ( 0.4485294117647058987, 0.4500000000000000111, 0.4529411764705882359, 0.4558823529411764608, 0.4588235294117646856, 0.4617647058823529660, 0.4632352941176470784 ),
 .UNSPECIFIED. ) 
 CURVE ( )  GEOMETRIC_REPRESENTATION_ITEM ( )  RATIONAL_B_SPLINE_CURVE ( ( 0.9755282581475768211, 0.9755282581475768211, 1.000000000000000000, 0.9510565162951535312, 1.000000000000000000, 0.9510565162951535312, 1.000000000000000000, 0.9510565162951535312, 1.000000000000000000, 0.9510565162951535312, 1.000000000000000000, 0.9755282581475768211, 0.9755282581475768211 ) ) 
 REPRESENTATION_ITEM ( '' )  );
#13834 = CARTESIAN_POINT ( 'NONE',  ( -151.4692556286852891, -196.9891397928655010, 40.65701158161630246 ) ) ;
#13835 = CARTESIAN_POINT ( 'NONE',  ( -54.92240467314265828, 790.2067769114943303, -0.8325491102011938205 ) ) ;
#13836 = CARTESIAN_POINT ( 'NONE',  ( 44.37947211624943833, 98.21518717409399812, 30.00020018409699318 ) ) ;
#13837 = CARTESIAN_POINT ( 'NONE',  ( 43.01140435219951286, 152.9604996726487798, 29.21067981925356705 ) ) ;
#13838 = CARTESIAN_POINT ( 'NONE',  ( 38.01140435219952707, 108.7104996726487514, 34.21067981925357060 ) ) ;
#13839 = CARTESIAN_POINT ( 'NONE',  ( -141.4692556286852891, -171.2130981290893033, 52.90620854394536821 ) ) ;
#13840 = CARTESIAN_POINT ( 'NONE',  ( 173.3794444120442506, -136.9891397928655010, -17.64809332337413750 ) ) ;
#13841 = CARTESIAN_POINT ( 'NONE',  ( 38.01140435219951996, 146.9344580088726104, 35.83527830041810347 ) ) ;
#13842 = CARTESIAN_POINT ( 'NONE',  ( 44.37947211624943833, 118.2797705074273296, 38.42115945441014446 ) ) ;
#13843 = CARTESIAN_POINT ( 'NONE',  ( 17.92634965299622252, 143.2997274935095788, 22.91961472066619265 ) ) ;
#13844 = CARTESIAN_POINT ( 'NONE',  ( 43.80332655382220253, 99.61133943119284595, 39.21067981925355639 ) ) ;
#13845 = CARTESIAN_POINT ( 'NONE',  ( 40.27526882409969744, 102.5651871740939924, 37.97664729208901235 ) ) ;
#13846 = EDGE_LOOP ( 'NONE', ( #8537, #8288, #5032, #13697 ) ) ;
#13847 = EDGE_CURVE ( 'NONE', #1905, #13229, #1633, .T. ) ;
#13848 = FACE_OUTER_BOUND ( 'NONE', #21516, .T. ) ;
#13849 = CARTESIAN_POINT ( 'NONE',  ( 10.61900875472251649, 108.8314319666055212, -5.279948415675857376 ) ) ;
#13850 = CARTESIAN_POINT ( 'NONE',  ( 71.20918238807936973, 120.1790618917378879, 12.65642078274776416 ) ) ;
#13851 = CARTESIAN_POINT ( 'NONE',  ( -151.4692556286852891, -196.9891397928655010, 59.65701158161632378 ) ) ;
#13852 = CARTESIAN_POINT ( 'NONE',  ( 38.58424406990786082, 90.37977050742732388, 34.21067981925357060 ) ) ;
#13853 = ORIENTED_EDGE ( 'NONE', *, *, #18788, .F. ) ;
#13854 = CARTESIAN_POINT ( 'NONE',  ( 47.05648932407426344, 76.58445800887257349, 31.27175355779120025 ) ) ;
#13855 = CARTESIAN_POINT ( 'NONE',  ( -141.4692556286852891, -171.8391397928654669, 46.40781461928724383 ) ) ;
#13856 = CARTESIAN_POINT ( 'NONE',  ( 43.01140435219951286, 130.4604996726487514, 39.46799094044489209 ) ) ;
#13858 = CARTESIAN_POINT ( 'NONE',  ( 71.68162264554656815, 101.3460857334412708, -13.77530061520655025 ) ) ;
#13857 = CARTESIAN_POINT ( 'NONE',  ( 46.59305225739526435, 91.31518717409399244, 36.81289934271958941 ) ) ;
#13859 = CARTESIAN_POINT ( 'NONE',  ( -157.2955611005346270, -158.6084106276440480, 41.63779006702063867 ) ) ;
#13860 = CARTESIAN_POINT ( 'NONE',  ( -145.6429501568359797, -177.8438272943106995, 57.67623309621197336 ) ) ;
#13861 = CARTESIAN_POINT ( 'NONE',  ( 43.01140435219951286, 116.0344580088725763, 29.21067981925356705 ) ) ;
#13862 = CARTESIAN_POINT ( 'NONE',  ( 116.4417310231185780, -126.9891397928655010, 49.65701158161629536 ) ) ;
#13863 = CARTESIAN_POINT ( 'NONE',  ( 39.92123440845005433, 80.33445800887258770, 29.95742577749336988 ) ) ;
#13864 = CARTESIAN_POINT ( 'NONE',  ( -158.9748091281504401, -116.9891397928655010, 62.65701158161630957 ) ) ;
#13865 = CARTESIAN_POINT ( 'NONE',  ( 121.4021762516569964, 137.5714195593754710, -19.99999999999997868 ) ) ;
#13866 = CARTESIAN_POINT ( 'NONE',  ( 43.01140435219951286, 151.1297705074273097, 38.86567161673127657 ) ) ;
#13867 = CARTESIAN_POINT ( 'NONE',  ( 38.58424406990784661, 102.2297705074273182, 32.77220824515698183 ) ) ;
#13868 = CARTESIAN_POINT ( 'NONE',  ( 74.61827669547474784, 133.2649018527303895, -2.855682626312802785 ) ) ;
#13869 = CARTESIAN_POINT ( 'NONE',  ( 41.64333658814960870, 134.5151871740939953, 30.00020018409699318 ) ) ;
#13870 = PLANE ( 'NONE',  #8625 ) ;
#13871 = CARTESIAN_POINT ( 'NONE',  ( -145.6429501568359797, -169.1084106276440480, 57.67623309621197336 ) ) ;
#13872 = CARTESIAN_POINT ( 'NONE',  ( 116.9721770337685740, 160.7104996726487798, -19.99999999999999289 ) ) ;
#13873 = AXIS2_PLACEMENT_3D ( 'NONE', #8815, #5592, #12319 ) ;
#13874 = CARTESIAN_POINT ( 'NONE',  ( 70.86003890729777766, 114.9808142912368254, 11.86642341732858874 ) ) ;
#13875 = CARTESIAN_POINT ( 'NONE',  ( 45.74753988029933538, 119.0651871740939782, 30.44471234641811819 ) ) ;
#13876 = AXIS2_PLACEMENT_3D ( 'NONE', #3532, #5288, #12002 ) ;
#13877 = ORIENTED_EDGE ( 'NONE', *, *, #10327, .T. ) ;
#13878 = CARTESIAN_POINT ( 'NONE',  ( 43.01140435219951286, 125.0344580088725905, 29.21067981925356705 ) ) ;
#13879 = ORIENTED_EDGE ( 'NONE', *, *, #9086, .T. ) ;
#13880 = CARTESIAN_POINT ( 'NONE',  ( 48.01140435219951996, 103.4344580088725536, 32.58608133808903773 ) ) ;
#13881 = CARTESIAN_POINT ( 'NONE',  ( 46.59305225739526435, 151.5797705074273267, 36.81289934271958941 ) ) ;
#13882 = CARTESIAN_POINT ( 'NONE',  ( 44.55648932407425633, 155.8104996726487741, 29.45539723777780239 ) ) ;
#13884 = CARTESIAN_POINT ( 'NONE',  ( 16.70103016558074316, 129.9804388327498827, 16.57432765154378629 ) ) ;
#13883 = CARTESIAN_POINT ( 'NONE',  ( 47.43856463449117200, 112.4651871740939839, 35.64915139335016647 ) ) ;
#13885 = EDGE_CURVE ( 'NONE', #20293, #11479, #17685, .T. ) ;
#13886 = AXIS2_PLACEMENT_3D ( 'NONE', #5808, #4478, #9350 ) ;
#13887 = CARTESIAN_POINT ( 'NONE',  ( 48.01140435219951996, 68.36049967264872862, 32.58608133808903773 ) ) ;
#13889 = CARTESIAN_POINT ( 'NONE',  ( 101.4021762516569822, 137.5714195593754710, 4.000000000000003553 ) ) ;
#13888 = CARTESIAN_POINT ( 'NONE',  ( -39.76538861119684753, -7.722638610254815461, -19.99999999999997868 ) ) ;
#13890 = DIRECTION ( 'NONE',  ( 1.000000000000000000, 0.000000000000000000, 0.000000000000000000 ) ) ;
#13891 = CARTESIAN_POINT ( 'NONE',  ( 46.98443111744539635, 95.22409955470565990, 37.26405200954400954 ) ) ;
#13892 =( BOUNDED_CURVE ( )  B_SPLINE_CURVE ( 2, ( #8034, #12874, #14305, #14627, #19820, #19595, #16387, #6036, #9690, #18154, #9358, #18043, #7817 ),
 .UNSPECIFIED., .F., .F. ) 
 B_SPLINE_CURVE_WITH_KNOTS ( ( 3, 2, 2, 2, 2, 2, 3 ),
 ( 0.09558823529411765441, 0.09705882352941176683, 0.1000000000000000056, 0.1029411764705882304, 0.1058823529411764691, 0.1088235294117647078, 0.1102941176470588203 ),
 .UNSPECIFIED. ) 
 CURVE ( )  GEOMETRIC_REPRESENTATION_ITEM ( )  RATIONAL_B_SPLINE_CURVE ( ( 0.9755282581475767101, 0.9755282581475768211, 1.000000000000000000, 0.9510565162951535312, 1.000000000000000000, 0.9510565162951535312, 1.000000000000000000, 0.9510565162951535312, 1.000000000000000000, 0.9510565162951535312, 1.000000000000000000, 0.9755282581475768211, 0.9755282581475767101 ) ) 
 REPRESENTATION_ITEM ( '' )  );
#13893 = CARTESIAN_POINT ( 'NONE',  ( 47.43856463449117200, 76.76518717409398107, 32.77220824515698183 ) ) ;
#13894 = CARTESIAN_POINT ( 'NONE',  ( -148.5561028927606344, -183.9938272943107336, 58.62277379824867296 ) ) ;
#13895 = CARTESIAN_POINT ( 'NONE',  ( -142.0420953463935803, -192.5084106276440252, 46.59394152635518083 ) ) ;
#13896 = VERTEX_POINT ( 'NONE', #6182 ) ;
#13897 = CARTESIAN_POINT ( 'NONE',  ( -148.5561028927606344, -177.0584106276440366, 40.69124936498395328 ) ) ;
#13898 = CARTESIAN_POINT ( 'NONE',  ( 8.916504151126011024, 123.7798070670463773, 8.215921583872152212 ) ) ;
#13899 = ORIENTED_EDGE ( 'NONE', *, *, #16655, .T. ) ;
#13900 = CARTESIAN_POINT ( 'NONE',  ( 45.74753988029933538, 143.0651871740939782, 30.44471234641811819 ) ) ;
#13901 = CARTESIAN_POINT ( 'NONE',  ( -130.4480969619997950, -126.9891397928655010, -72.64809332337412684 ) ) ;
#13902 = CARTESIAN_POINT ( 'NONE',  ( 43.01140435219951286, 104.6297705074273239, 29.55568802177586107 ) ) ;
#13903 = CARTESIAN_POINT ( 'NONE',  ( 20.88913110926514705, 146.0313881486468119, 3.053432864643822686 ) ) ;
#13904 = ORIENTED_EDGE ( 'NONE', *, *, #15318, .T. ) ;
#13905 = CARTESIAN_POINT ( 'NONE',  ( 68.29827362630597065, 132.3882971431532383, 5.156253003121209488 ) ) ;
#13906 = ORIENTED_EDGE ( 'NONE', *, *, #13052, .T. ) ;
#13907 = CARTESIAN_POINT ( 'NONE',  ( 47.43856463449118621, 112.8797705074273097, 34.21067981925357060 ) ) ;
#13908 = DIRECTION ( 'NONE',  ( 0.000000000000000000, 0.000000000000000000, 1.000000000000000000 ) ) ;
#13909 = CARTESIAN_POINT ( 'NONE',  ( 43.01140435219951286, 88.46049967264873715, 39.21067981925356349 ) ) ;
#13910 = VECTOR ( 'NONE', #12289, 1000.000000000000000 ) ;
#13911 = CARTESIAN_POINT ( 'NONE',  ( 43.01140435219951286, 149.3651871740939612, 29.55568802177586463 ) ) ;
#13912 = CARTESIAN_POINT ( 'NONE',  ( 38.96631938032478359, 106.0104996726487485, 37.14960608071593384 ) ) ;
#13913 = CARTESIAN_POINT ( 'NONE',  ( 9.021810916323596885, 123.9851095102452945, 2.220310480865780534 ) ) ;
#13914 = CARTESIAN_POINT ( 'NONE',  ( 38.01140435219952707, 60.71049967264874425, 34.21067981925357060 ) ) ;
#13915 = CARTESIAN_POINT ( 'NONE',  ( -157.6495955161842062, -170.9391397928654328, 41.15050349809590102 ) ) ;
#13916 = CARTESIAN_POINT ( 'NONE',  ( -151.4692556286852891, -196.9891397928655010, 49.65701158161630957 ) ) ;
#13917 = CARTESIAN_POINT ( 'NONE',  ( -47.86331837773882825, -37.13255853780189852, -19.99999999999997158 ) ) ;
#13918 = APPLICATION_CONTEXT ( 'automotive_design' ) ;
#13919 = DIRECTION ( 'NONE',  ( -0.000000000000000000, 1.000000000000000000, -0.000000000000000000 ) ) ;
#13920 = EDGE_CURVE ( 'NONE', #14777, #9423, #1122, .T. ) ;
#13921 = CARTESIAN_POINT ( 'NONE',  ( 40.27526882409969033, 86.92977050742732104, 30.44471234641811819 ) ) ;
#13922 = CARTESIAN_POINT ( 'NONE',  ( -157.2955611005346270, -163.4438272943107506, 57.67623309621198047 ) ) ;
#13923 = EDGE_CURVE ( 'NONE', #15014, #19018, #4889, .T. ) ;
#13924 = CARTESIAN_POINT ( 'NONE',  ( 40.27526882409969744, 78.56518717409399244, 37.97664729208901235 ) ) ;
#13925 = CARTESIAN_POINT ( 'NONE',  ( -151.4692556286852891, -126.9891397928655010, -54.65701158161630246 ) ) ;
#13926 = CARTESIAN_POINT ( 'NONE',  ( 43.01140435219951996, 10.71049967264875491, 34.21067981925357060 ) ) ;
#13927 = ORIENTED_EDGE ( 'NONE', *, *, #13155, .F. ) ;
#13928 = CARTESIAN_POINT ( 'NONE',  ( 48.01140435219951996, 85.13445800887258486, 35.83527830041809636 ) ) ;
#13929 = CARTESIAN_POINT ( 'NONE',  ( 173.3794444120442506, -84.13255853780189852, 20.00000000000001776 ) ) ;
#13930 = CARTESIAN_POINT ( 'NONE',  ( 44.37947211624943833, 130.2797705074273154, 38.42115945441014446 ) ) ;
#13931 = CARTESIAN_POINT ( 'NONE',  ( 74.95715479139145998, 107.8263973513541742, -14.01376907723217613 ) ) ;
#13932 = EDGE_LOOP ( 'NONE', ( #16264, #19632, #18865, #6459 ) ) ;
#13933 = CARTESIAN_POINT ( 'NONE',  ( 43.01140435219951286, 72.53445800887256212, 39.21067981925356349 ) ) ;
#13934 = ORIENTED_EDGE ( 'NONE', *, *, #3727, .T. ) ;
#13935 = CARTESIAN_POINT ( 'NONE',  ( 45.74753988029933538, 140.3297705074272983, 30.44471234641811819 ) ) ;
#13936 = CARTESIAN_POINT ( 'NONE',  ( 38.58424406990784661, 93.22977050742730398, 32.77220824515698183 ) ) ;
#13937 = CARTESIAN_POINT ( 'NONE',  ( -148.3790856849358306, -180.3891397928654783, 40.14644641866477315 ) ) ;
#13938 = DIRECTION ( 'NONE',  ( 1.000000000000000000, 0.000000000000000000, -2.229410185538112728E-16 ) ) ;
#13939 = CARTESIAN_POINT ( 'NONE',  ( 43.01140435219951286, 90.53445800887257633, 39.21067981925356349 ) ) ;
#13940 = CARTESIAN_POINT ( 'NONE',  ( 163.1802725128760585, 192.2118331161914568, 24.05341166118710561 ) ) ;
#13941 = VECTOR ( 'NONE', #8339, 1000.000000000000000 ) ;
#13942 = CARTESIAN_POINT ( 'NONE',  ( 46.59305225739526435, 97.91518717409400097, 31.60846029578754468 ) ) ;
#13943 = DIRECTION ( 'NONE',  ( -0.000000000000000000, -0.000000000000000000, 1.000000000000000000 ) ) ;
#13944 = DIRECTION ( 'NONE',  ( 1.000000000000000000, 0.000000000000000000, 0.000000000000000000 ) ) ;
#13945 = CARTESIAN_POINT ( 'NONE',  ( -159.5594255724347761, -157.2630981290893146, 55.53486410454104316 ) ) ;
#13946 = DIRECTION ( 'NONE',  ( 0.000000000000000000, 0.000000000000000000, 1.000000000000000000 ) ) ;
#13947 = CARTESIAN_POINT ( 'NONE',  ( 43.01140435219951286, 141.5344580088725763, 39.46799094044489209 ) ) ;
#13948 = CARTESIAN_POINT ( 'NONE',  ( 47.43856463449117200, 113.0297705074273011, 32.77220824515698183 ) ) ;
#13949 = CARTESIAN_POINT ( 'NONE',  ( 49.69400319086401652, 86.25038505451357196, 20.12058643263999969 ) ) ;
#13950 = CARTESIAN_POINT ( 'NONE',  ( -151.4692556286853176, -179.3130981290892976, 39.65701158161629536 ) ) ;
#13951 = CARTESIAN_POINT ( 'NONE',  ( 39.42975644700377558, 108.4151871740940152, 36.81289934271958941 ) ) ;
#13952 = ORIENTED_EDGE ( 'NONE', *, *, #8265, .F. ) ;
#13953 = FACE_OUTER_BOUND ( 'NONE', #17131, .T. ) ;
#13954 = CARTESIAN_POINT ( 'NONE',  ( 12.59043673732666946, 104.3826120832696773, 9.557940159192295226 ) ) ;
#13955 = VECTOR ( 'NONE', #12176, 1000.000000000000000 ) ;
#13956 = CARTESIAN_POINT ( 'NONE',  ( 70.94289844336020678, 123.7826807253454575, 5.513563639855703080 ) ) ;
#13957 = DIRECTION ( 'NONE',  ( -0.3450121214752274734, 0.9385982292947089300, 0.000000000000000000 ) ) ;
#13958 = CARTESIAN_POINT ( 'NONE',  ( 47.43856463449118621, 76.87977050742732388, 34.21067981925357060 ) ) ;
#13959 =( BOUNDED_CURVE ( )  B_SPLINE_CURVE ( 2, ( #20481, #5372, #3724, #308, #18818, #7036, #11876, #8253, #11764, #10126, #13634, #13425, #191 ),
 .UNSPECIFIED., .F., .F. ) 
 B_SPLINE_CURVE_WITH_KNOTS ( ( 3, 2, 2, 2, 2, 2, 3 ),
 ( 0.9107142857142856984, 0.9142857142857142572, 0.9214285714285713746, 0.9285714285714286031, 0.9357142857142857206, 0.9428571428571428381, 0.9464285714285713969 ),
 .UNSPECIFIED. ) 
 CURVE ( )  GEOMETRIC_REPRESENTATION_ITEM ( )  RATIONAL_B_SPLINE_CURVE ( ( 0.9755282581475768211, 0.9755282581475768211, 1.000000000000000000, 0.9510565162951535312, 1.000000000000000000, 0.9510565162951535312, 1.000000000000000000, 0.9510565162951535312, 1.000000000000000000, 0.9510565162951535312, 1.000000000000000000, 0.9755282581475768211, 0.9755282581475768211 ) ) 
 REPRESENTATION_ITEM ( '' )  );
#13960 = ORIENTED_EDGE ( 'NONE', *, *, #20210, .T. ) ;
#13961 = CARTESIAN_POINT ( 'NONE',  ( 38.01140435219951996, 65.93445800887258201, 35.83527830041810347 ) ) ;
#13962 = DIRECTION ( 'NONE',  ( 0.000000000000000000, 0.000000000000000000, 1.000000000000000000 ) ) ;
#13963 = CARTESIAN_POINT ( 'NONE',  ( 38.96631938032478359, 127.0104996726487343, 37.14960608071593384 ) ) ;
#13965 = CARTESIAN_POINT ( 'NONE',  ( 37.47668497174467461, 153.6095807538456199, -2.346729193546184700 ) ) ;
#13964 = CARTESIAN_POINT ( 'NONE',  ( 47.43856463449118621, 91.61518717409400381, 34.21067981925357060 ) ) ;
#13966 = VECTOR ( 'NONE', #7994, 1000.000000000000000 ) ;
#13967 = CARTESIAN_POINT ( 'NONE',  ( -145.6429501568359797, -182.9438272943107222, 41.63779006702063867 ) ) ;
#13968 = CARTESIAN_POINT ( 'NONE',  ( 38.01140435219952707, 116.7844580088725763, 34.21067981925357060 ) ) ;
#13969 = PLANE ( 'NONE',  #7210 ) ;
#13970 = CARTESIAN_POINT ( 'NONE',  ( 43.01140435219951286, 80.03445800887257633, 29.21067981925356705 ) ) ;
#13971 = PLANE ( 'NONE',  #13873 ) ;
#13972 = CARTESIAN_POINT ( 'NONE',  ( 43.01140435219951286, 143.9604996726487229, 29.21067981925356705 ) ) ;
#13973 = CARTESIAN_POINT ( 'NONE',  ( 39.42975644700377558, 144.6797705074273495, 36.81289934271958941 ) ) ;
#13974 = CARTESIAN_POINT ( 'NONE',  ( 40.27526882409969033, 107.9297705074273352, 30.44471234641811819 ) ) ;
#13975 = CARTESIAN_POINT ( 'NONE',  ( 14.15704070161504369, 138.3271338521546454, 9.720138693322796897 ) ) ;
#13976 = CARTESIAN_POINT ( 'NONE',  ( 41.64333658814960870, 140.5151871740939953, 30.00020018409699318 ) ) ;
#13977 = CARTESIAN_POINT ( 'NONE',  ( -142.0420953463936087, -156.3938272943107393, 49.65701158161630957 ) ) ;
#13978 = CARTESIAN_POINT ( 'NONE',  ( -159.0959885057557983, -161.4584106276440423, 44.11586579668791330 ) ) ;
#13979 = CARTESIAN_POINT ( 'NONE',  ( 111.4021762516569964, 137.5714195593754710, -19.99999999999997868 ) ) ;
#13980 = CARTESIAN_POINT ( 'NONE',  ( 44.55648932407425633, 90.68445800887258201, 38.96596240072933170 ) ) ;
#13981 = CARTESIAN_POINT ( 'NONE',  ( 58.30185729850432352, 143.6975816885063750, 10.55682690296339032 ) ) ;
#13982 = VECTOR ( 'NONE', #5759, 1000.000000000000000 ) ;
#13983 = CARTESIAN_POINT ( 'NONE',  ( -151.4692556286852891, -187.7391397928655010, 59.65701158161632378 ) ) ;
#13984 = CARTESIAN_POINT ( 'NONE',  ( 40.27526882409969033, 116.6651871740939868, 30.44471234641811819 ) ) ;
#13985 = VERTEX_POINT ( 'NONE', #3544 ) ;
#13986 = AXIS2_PLACEMENT_3D ( 'NONE', #9297, #803, #9083 ) ;
#13987 = CARTESIAN_POINT ( 'NONE',  ( -161.4692556286852891, -179.3391397928654669, 52.90620854394536821 ) ) ;
#13988 = EDGE_LOOP ( 'NONE', ( #2653, #1927, #5990, #18579 ) ) ;
#13989 = CARTESIAN_POINT ( 'NONE',  ( 48.01140435219951996, 91.43445800887258201, 32.58608133808903773 ) ) ;
#13990 = EDGE_CURVE ( 'NONE', #137, #17423, #15184, .T. ) ;
#13991 = CARTESIAN_POINT ( 'NONE',  ( 41.64333658814960870, 146.7797705074273154, 30.00020018409699318 ) ) ;
#13992 = CARTESIAN_POINT ( 'NONE',  ( 38.58424406990786082, 60.37977050742732388, 34.21067981925357060 ) ) ;
#13994 = CARTESIAN_POINT ( 'NONE',  ( 59.36841858216658352, 96.93634223693318575, 13.72768157422830981 ) ) ;
#13993 = CARTESIAN_POINT ( 'NONE',  ( 46.59305225739526435, 118.3151871740940067, 36.81289934271958941 ) ) ;
#13995 = VECTOR ( 'NONE', #3934, 1000.000000000000000 ) ;
#13996 = CARTESIAN_POINT ( 'NONE',  ( 48.01140435219951996, 68.21049967264873715, 34.21067981925357060 ) ) ;
#13998 = CYLINDRICAL_SURFACE ( 'NONE', #6183, 4.999999999999997335 ) ;
#13997 = CARTESIAN_POINT ( 'NONE',  ( 41.46631938032478359, 108.3844580088725849, 38.96596240072933170 ) ) ;
#13999 = AXIS2_PLACEMENT_3D ( 'NONE', #12957, #21783, #13397 ) ;
#14000 = CARTESIAN_POINT ( 'NONE',  ( -153.0531000319307111, -173.2362167067690564, 39.65701158161631668 ) ) ;
#14001 = CARTESIAN_POINT ( 'NONE',  ( 46.31788101060713814, 95.12560940527907860, 37.97538637126936578 ) ) ;
#14002 = CARTESIAN_POINT ( 'NONE',  ( 38.58424406990786082, 72.11518717409400381, 34.21067981925357060 ) ) ;
#14003 = CARTESIAN_POINT ( 'NONE',  ( 39.92123440845005433, 64.16049967264873999, 38.46393386101375711 ) ) ;
#14004 = CARTESIAN_POINT ( 'NONE',  ( -157.2955611005346270, -185.3438272943106995, 41.63779006702063867 ) ) ;
#14005 = CARTESIAN_POINT ( 'NONE',  ( -157.2955611005345986, -191.6084106276440480, 41.63779006702063867 ) ) ;
#14006 = VERTEX_POINT ( 'NONE', #15335 ) ;
#14007 = CARTESIAN_POINT ( 'NONE',  ( -160.8964159109769696, -176.0084106276440536, 52.72008163687743121 ) ) ;
#14008 = CARTESIAN_POINT ( 'NONE',  ( 76.90526227772885193, 114.5556580205831096, 4.763324653225488703 ) ) ;
#14009 = EDGE_CURVE ( 'NONE', #18451, #40, #6965, .T. ) ;
#14010 = ORIENTED_EDGE ( 'NONE', *, *, #13768, .F. ) ;
#14011 = CARTESIAN_POINT ( 'NONE',  ( 41.64333658814960870, 141.7151871740940123, 38.42115945441014446 ) ) ;
#14012 = DIRECTION ( 'NONE',  ( -0.7067093775913396714, 0.7073806645723093034, -0.01320799052465169467 ) ) ;
#14013 = CARTESIAN_POINT ( 'NONE',  ( 44.37947211624943833, 107.4797705074273182, 30.00020018409699318 ) ) ;
#14014 = CARTESIAN_POINT ( 'NONE',  ( 61.01612483116806374, 90.79174121657607088, -0.2798613066081144796 ) ) ;
#14015 = ORIENTED_EDGE ( 'NONE', *, *, #305, .T. ) ;
#14016 = CARTESIAN_POINT ( 'NONE',  ( 15.00983914341701997, 123.2415857317943448, 2.299110145932334426 ) ) ;
#14017 = ORIENTED_EDGE ( 'NONE', *, *, #9609, .T. ) ;
#14018 = CARTESIAN_POINT ( 'NONE',  ( 43.01140435219951286, 112.1297705074272812, 38.86567161673127657 ) ) ;
#14019 = DIRECTION ( 'NONE',  ( 1.000000000000000000, 0.000000000000000000, 0.000000000000000000 ) ) ;
#14020 = CARTESIAN_POINT ( 'NONE',  ( 40.27526882409969033, 149.6651871740939725, 30.44471234641811819 ) ) ;
#14021 =( BOUNDED_SURFACE ( )  B_SPLINE_SURFACE ( 1, 2, ( 
 ( #2355, #14035, #10637, #6089, #17341, #9094, #14359, #916, #5983, #7662, #5661, #12384, #12710, #19119, #4014, #19433, #17662, #15795, #17551, #705, #7438, #14141, #20878, #5766, #12495, #2460, #9200, #19221, #4119, #12604, #15898, #810, #7547, #20989, #5874, #11162, #21753, #19877, #2787, #19997, #4881, #9850, #21648, #6426, #6539, #8305, #9529, #16226, #3230, #13260, #1137, #11485, #11600, #15013, #16552, #18330, #17986, #14571, #18214, #7872, #4546, #4430, #2900, #17875, #3119, #21313, #1577, #13148, #9963, #16666, #1467, #12930, #9745, #12817, #6198, #4764, #7978, #19536, #19654, #3008, #11267, #14900, #14685, #8199, #9635, #16335, #21425, #16442, #1244, #6314, #13041, #19765, #4662, #11377, #18098, #1356, #8087, #14794, #21536, #3561, #8743, #8633, #15352, #16778, #1897, #8418, #20421, #13791, #18442, #6663, #15128, #6769, #15460, #16882, #31, #10396, #13579, #11707, #20107, #15243, #10285, #3458, #5104, #18765, #13370, #13478, #3666, #6872, #246, #10069, #360, #20316, #17096, #2012, #7088, #4996, #3341, #1688, #20211, #6984, #10181, #8530, #11820, #18552, #12031, #1799, #141, #5214, #11928, #18657, #16990, #13687, #5318, #8153, #17945, #19721, #2962, #4954, #14966, #14858, #11662, #6269, #4502, #16402, #14752, #3299, #21493, #13000, #9594, #9918, #1425, #13331, #16733, #18286, #13214, #6615, #2851, #11225, #20067, #6380, #11442, #8376, #18400, #10027, #1644, #21605, #13436, #8048, #13110, #16624, #9702, #3189, #4613, #1313, #19832, #15085, #14775, #6730, #4722, #19951, #16295, #6495, #11334, #1533, #18167, #3075, #14640, #9812, #16508, #1201, #21713, #8266, #4836, #7936, #21382, #11558, #18055, #10139, #15422, #3521, #15521, #20381, #17165, #10247, #102, #3735, #8490, #11888, #11777, #16945, #3417, #10465, #6834, #8917, #20492, #17270, #10569, #2079, #20275, #17056, #15620, #18506, #5381, #15310, #7562, #2182, #10353, #13859, #424, #202, #12096, #826, #3842, #6941, #1968, #7156, #13647, #16842, #5168, #18829, #1861, #20174, #1755, #8810, #5278, #317, #8702, #7046, #15199 ),
 ( #13540, #5482, #11992, #18722, #13752, #20596, #12207, #5064, #18617, #18942, #8591, #3629, #21006, #16021, #7677, #21439, #11284, #7887, #5996, #4240, #14260, #18114, #3025, #12726, #9650, #18004, #16351, #4563, #9760, #17678, #1260, #16458, #10966, #2916, #12947, #14375, #6104, #4675, #2690, #6330, #2581, #14702, #7997, #12834, #19552, #9319, #9434, #14588, #933, #4448, #13056, #2804, #21114, #12619, #1370, #21331, #19449, #19782, #11391, #5888, #19340, #6216, #4342, #11068, #17782, #16137, #1046, #7780, #14480, #19669, #21224, #11178, #17891, #9542, #16244, #1152, #3474, #11946, #14809, #16901, #10198, #20016, #21551, #9867, #1485, #15259, #5120, #1706, #21666, #19895, #8102, #18676, #3578, #6557, #1814, #11838, #8547, #20228, #10305, #11504, #157, #17007, #4784, #18568, #6790, #8217, #21773, #20334, #18347, #6889, #18234, #13596, #5231, #6679, #13388, #3136, #3250, #8436, #16566, #20123, #6442, #18458, #14916, #13164, #13281, #15145, #4900, #11619, #9979, #16683, #1593, #45, #8324, #15034, #5016, #11724, #3359, #10084, #16794, #13495, #10734, #4109, #5652, #15787, #7106, #3683, #7325, #12050, #15476, #15372, #13811, #7000, #14026, #10411, #12485, #2239, #20868, #14129, #20759, #2029, #20654, #19212, #265, #8973, #18885, #10845, #5756, #13915, #17435, #4005, #3793, #15678, #1915, #7429, #10522, #5538, #2343, #17217, #13704, #8759, #582, #20549, #8650, #20440, #12370, #2135, #3901, #12265, #10625, #5332, #377, #19110, #9081, #694, #18779, #17332, #17113, #5432, #12152, #8867, #15575, #479, #7215, #19000, #4423, #12701, #7652, #11256, #19756, #4216, #19645, #2661, #17868, #7536, #1234, #9406, #4536, #17977, #2888, #4650, #6304, #21305, #7864, #17759, #802, #5866, #21196, #6189, #11043, #16115, #11153, #2780, #15997, #17542, #9626, #9520, #16325, #6082, #9192, #10946, #907, #7969, #12920, #12809, #14675, #19318, #2451, #14351, #5973, #13032, #19422, #17653, #14239, #1129, #14456, #15889, #20978, #16219, #14563, #12597, #2559, #9296, #21092, #4319, #1021, #7757, #19529, #16873, #10173 ) ),
 .UNSPECIFIED., .F., .F., .F. ) 
 B_SPLINE_SURFACE_WITH_KNOTS ( ( 2, 2 ),
 ( 3, 2, 2, 2, 2, 2, 2, 2, 2, 2, 2, 2, 2, 2, 2, 2, 2, 2, 2, 2, 2, 2, 2, 2, 2, 2, 2, 2, 2, 2, 2, 2, 2, 2, 2, 2, 2, 2, 2, 2, 2, 2, 2, 2, 2, 2, 2, 2, 2, 2, 2, 2, 2, 2, 2, 2, 2, 2, 2, 2, 2, 2, 2, 2, 2, 2, 2, 2, 2, 2, 2, 2, 2, 2, 2, 2, 2, 2, 2, 2, 2, 2, 2, 2, 2, 2, 2, 2, 2, 2, 2, 2, 2, 2, 2, 2, 2, 2, 2, 2, 2, 2, 2, 2, 2, 2, 2, 2, 2, 2, 2, 2, 2, 2, 2, 2, 2, 2, 2, 2, 2, 2, 2, 2, 2, 2, 2, 2, 2, 2, 2, 2, 2, 2, 3 ),
 ( 0.000000000000000000, 1.000000000000000000 ),
 ( 0.000000000000000000, 0.007142857142857142634, 0.01428571428571428527, 0.02142857142857142877, 0.02857142857142857054, 0.03571428571428571230, 0.04285714285714285754, 0.05000000000000000278, 0.05714285714285714107, 0.06428571428571427937, 0.07142857142857142461, 0.07857142857142856984, 0.08571428571428571508, 0.09285714285714286031, 0.1000000000000000056, 0.1071428571428571369, 0.1142857142857142821, 0.1214285714285714274, 0.1285714285714285587, 0.1357142857142857040, 0.1428571428571428492, 0.1499999999999999944, 0.1571428571428571397, 0.1642857142857142849, 0.1714285714285714302, 0.1785714285714285754, 0.1857142857142857206, 0.1928571428571428659, 0.2000000000000000111, 0.2071428571428571563, 0.2142857142857142738, 0.2214285714285714191, 0.2285714285714285643, 0.2357142857142857095, 0.2428571428571428548, 0.2500000000000000000, 0.2571428571428571175, 0.2642857142857142905, 0.2714285714285714080, 0.2785714285714285809, 0.2857142857142856984, 0.2928571428571428714, 0.2999999999999999889, 0.3071428571428571619, 0.3142857142857142794, 0.3214285714285714524, 0.3285714285714285698, 0.3357142857142856873, 0.3428571428571428603, 0.3499999999999999778, 0.3571428571428571508, 0.3642857142857142683, 0.3714285714285714413, 0.3785714285714285587, 0.3857142857142857317, 0.3928571428571428492, 0.4000000000000000222, 0.4071428571428571397, 0.4142857142857143127, 0.4214285714285714302, 0.4285714285714285476, 0.4357142857142857206, 0.4428571428571428381, 0.4500000000000000111, 0.4571428571428571286, 0.4642857142857143016, 0.4714285714285714191, 0.4785714285714285920, 0.4857142857142857095, 0.4928571428571428825, 0.5000000000000000000, 0.5071428571428571175, 0.5142857142857142350, 0.5214285714285714635, 0.5285714285714285809, 0.5357142857142856984, 0.5428571428571428159, 0.5500000000000000444, 0.5571428571428571619, 0.5642857142857142794, 0.5714285714285713969, 0.5785714285714286254, 0.5857142857142857428, 0.5928571428571428603, 0.5999999999999999778, 0.6071428571428570953, 0.6142857142857143238, 0.6214285714285714413, 0.6285714285714285587, 0.6357142857142856762, 0.6428571428571429047, 0.6500000000000000222, 0.6571428571428571397, 0.6642857142857142572, 0.6714285714285713746, 0.6785714285714286031, 0.6857142857142857206, 0.6928571428571428381, 0.6999999999999999556, 0.7071428571428571841, 0.7142857142857143016, 0.7214285714285714191, 0.7285714285714285365, 0.7357142857142857650, 0.7428571428571428825, 0.7500000000000000000, 0.7571428571428571175, 0.7642857142857142350, 0.7714285714285714635, 0.7785714285714285809, 0.7857142857142856984, 0.7928571428571428159, 0.8000000000000000444, 0.8071428571428571619, 0.8142857142857142794, 0.8214285714285713969, 0.8285714285714286254, 0.8357142857142857428, 0.8428571428571428603, 0.8499999999999999778, 0.8571428571428570953, 0.8642857142857143238, 0.8714285714285714413, 0.8785714285714285587, 0.8857142857142856762, 0.8928571428571429047, 0.9000000000000000222, 0.9071428571428571397, 0.9142857142857142572, 0.9214285714285713746, 0.9285714285714286031, 0.9357142857142857206, 0.9428571428571428381, 0.9499999999999999556, 0.9523897249335829818 ),
 .UNSPECIFIED. ) 
 GEOMETRIC_REPRESENTATION_ITEM ( )  RATIONAL_B_SPLINE_SURFACE ( (
 ( 1.000000000000000000, 0.9510565162951535312, 1.000000000000000000, 0.9510565162951535312, 1.000000000000000000, 0.9510565162951535312, 1.000000000000000000, 0.9510565162951535312, 1.000000000000000000, 0.9510565162951535312, 1.000000000000000000, 0.9510565162951535312, 1.000000000000000000, 0.9510565162951535312, 1.000000000000000000, 0.9510565162951535312, 1.000000000000000000, 0.9510565162951535312, 1.000000000000000000, 0.9510565162951535312, 1.000000000000000000, 0.9510565162951535312, 1.000000000000000000, 0.9510565162951535312, 1.000000000000000000, 0.9510565162951535312, 1.000000000000000000, 0.9510565162951535312, 1.000000000000000000, 0.9510565162951535312, 1.000000000000000000, 0.9510565162951535312, 1.000000000000000000, 0.9510565162951535312, 1.000000000000000000, 0.9510565162951535312, 1.000000000000000000, 0.9510565162951535312, 1.000000000000000000, 0.9510565162951535312, 1.000000000000000000, 0.9510565162951535312, 1.000000000000000000, 0.9510565162951535312, 1.000000000000000000, 0.9510565162951535312, 1.000000000000000000, 0.9510565162951535312, 1.000000000000000000, 0.9510565162951535312, 1.000000000000000000, 0.9510565162951535312, 1.000000000000000000, 0.9510565162951535312, 1.000000000000000000, 0.9510565162951535312, 1.000000000000000000, 0.9510565162951535312, 1.000000000000000000, 0.9510565162951535312, 1.000000000000000000, 0.9510565162951535312, 1.000000000000000000, 0.9510565162951535312, 1.000000000000000000, 0.9510565162951535312, 1.000000000000000000, 0.9510565162951535312, 1.000000000000000000, 0.9510565162951535312, 1.000000000000000000, 0.9510565162951535312, 1.000000000000000000, 0.9510565162951535312, 1.000000000000000000, 0.9510565162951535312, 1.000000000000000000, 0.9510565162951535312, 1.000000000000000000, 0.9510565162951535312, 1.000000000000000000, 0.9510565162951535312, 1.000000000000000000, 0.9510565162951535312, 1.000000000000000000, 0.9510565162951535312, 1.000000000000000000, 0.9510565162951535312, 1.000000000000000000, 0.9510565162951535312, 1.000000000000000000, 0.9510565162951535312, 1.000000000000000000, 0.9510565162951535312, 1.000000000000000000, 0.9510565162951535312, 1.000000000000000000, 0.9510565162951535312, 1.000000000000000000, 0.9510565162951535312, 1.000000000000000000, 0.9510565162951535312, 1.000000000000000000, 0.9510565162951535312, 1.000000000000000000, 0.9510565162951535312, 1.000000000000000000, 0.9510565162951535312, 1.000000000000000000, 0.9510565162951535312, 1.000000000000000000, 0.9510565162951535312, 1.000000000000000000, 0.9510565162951535312, 1.000000000000000000, 0.9510565162951535312, 1.000000000000000000, 0.9510565162951535312, 1.000000000000000000, 0.9510565162951535312, 1.000000000000000000, 0.9510565162951535312, 1.000000000000000000, 0.9510565162951535312, 1.000000000000000000, 0.9510565162951535312, 1.000000000000000000, 0.9510565162951535312, 1.000000000000000000, 0.9510565162951535312, 1.000000000000000000, 0.9510565162951535312, 1.000000000000000000, 0.9510565162951535312, 1.000000000000000000, 0.9510565162951535312, 1.000000000000000000, 0.9510565162951535312, 1.000000000000000000, 0.9510565162951535312, 1.000000000000000000, 0.9510565162951535312, 1.000000000000000000, 0.9510565162951535312, 1.000000000000000000, 0.9510565162951535312, 1.000000000000000000, 0.9510565162951535312, 1.000000000000000000, 0.9510565162951535312, 1.000000000000000000, 0.9510565162951535312, 1.000000000000000000, 0.9510565162951535312, 1.000000000000000000, 0.9510565162951535312, 1.000000000000000000, 0.9510565162951535312, 1.000000000000000000, 0.9510565162951535312, 1.000000000000000000, 0.9510565162951535312, 1.000000000000000000, 0.9510565162951535312, 1.000000000000000000, 0.9510565162951535312, 1.000000000000000000, 0.9510565162951535312, 1.000000000000000000, 0.9510565162951535312, 1.000000000000000000, 0.9510565162951535312, 1.000000000000000000, 0.9510565162951535312, 1.000000000000000000, 0.9510565162951535312, 1.000000000000000000, 0.9510565162951535312, 1.000000000000000000, 0.9510565162951535312, 1.000000000000000000, 0.9510565162951535312, 1.000000000000000000, 0.9510565162951535312, 1.000000000000000000, 0.9510565162951535312, 1.000000000000000000, 0.9510565162951535312, 1.000000000000000000, 0.9510565162951535312, 1.000000000000000000, 0.9510565162951535312, 1.000000000000000000, 0.9510565162951535312, 1.000000000000000000, 0.9510565162951535312, 1.000000000000000000, 0.9510565162951535312, 1.000000000000000000, 0.9510565162951535312, 1.000000000000000000, 0.9510565162951535312, 1.000000000000000000, 0.9510565162951535312, 1.000000000000000000, 0.9510565162951535312, 1.000000000000000000, 0.9510565162951535312, 1.000000000000000000, 0.9510565162951535312, 1.000000000000000000, 0.9510565162951535312, 1.000000000000000000, 0.9510565162951535312, 1.000000000000000000, 0.9510565162951535312, 1.000000000000000000, 0.9510565162951535312, 1.000000000000000000, 0.9510565162951535312, 1.000000000000000000, 0.9510565162951535312, 1.000000000000000000, 0.9510565162951535312, 1.000000000000000000, 0.9510565162951535312, 1.000000000000000000, 0.9510565162951535312, 1.000000000000000000, 0.9510565162951535312, 1.000000000000000000, 0.9510565162951535312, 1.000000000000000000, 0.9510565162951535312, 1.000000000000000000, 0.9510565162951535312, 1.000000000000000000, 0.9510565162951535312, 1.000000000000000000, 0.9510565162951535312, 1.000000000000000000, 0.9510565162951535312, 1.000000000000000000, 0.9510565162951535312, 1.000000000000000000, 0.9510565162951535312, 1.000000000000000000, 0.9510565162951535312, 1.000000000000000000, 0.9510565162951535312, 1.000000000000000000, 0.9510565162951535312, 1.000000000000000000, 0.9510565162951535312, 1.000000000000000000, 0.9510565162951535312, 1.000000000000000000, 0.9510565162951535312, 1.000000000000000000, 0.9510565162951535312, 1.000000000000000000, 0.9510565162951535312, 1.000000000000000000, 0.9510565162951535312, 1.000000000000000000, 0.9510565162951535312, 1.000000000000000000, 0.9836253951315760968, 0.9782074146920120006),
 ( 1.000000000000000000, 0.9510565162951535312, 1.000000000000000000, 0.9510565162951535312, 1.000000000000000000, 0.9510565162951535312, 1.000000000000000000, 0.9510565162951535312, 1.000000000000000000, 0.9510565162951535312, 1.000000000000000000, 0.9510565162951535312, 1.000000000000000000, 0.9510565162951535312, 1.000000000000000000, 0.9510565162951535312, 1.000000000000000000, 0.9510565162951535312, 1.000000000000000000, 0.9510565162951535312, 1.000000000000000000, 0.9510565162951535312, 1.000000000000000000, 0.9510565162951535312, 1.000000000000000000, 0.9510565162951535312, 1.000000000000000000, 0.9510565162951535312, 1.000000000000000000, 0.9510565162951535312, 1.000000000000000000, 0.9510565162951535312, 1.000000000000000000, 0.9510565162951535312, 1.000000000000000000, 0.9510565162951535312, 1.000000000000000000, 0.9510565162951535312, 1.000000000000000000, 0.9510565162951535312, 1.000000000000000000, 0.9510565162951535312, 1.000000000000000000, 0.9510565162951535312, 1.000000000000000000, 0.9510565162951535312, 1.000000000000000000, 0.9510565162951535312, 1.000000000000000000, 0.9510565162951535312, 1.000000000000000000, 0.9510565162951535312, 1.000000000000000000, 0.9510565162951535312, 1.000000000000000000, 0.9510565162951535312, 1.000000000000000000, 0.9510565162951535312, 1.000000000000000000, 0.9510565162951535312, 1.000000000000000000, 0.9510565162951535312, 1.000000000000000000, 0.9510565162951535312, 1.000000000000000000, 0.9510565162951535312, 1.000000000000000000, 0.9510565162951535312, 1.000000000000000000, 0.9510565162951535312, 1.000000000000000000, 0.9510565162951535312, 1.000000000000000000, 0.9510565162951535312, 1.000000000000000000, 0.9510565162951535312, 1.000000000000000000, 0.9510565162951535312, 1.000000000000000000, 0.9510565162951535312, 1.000000000000000000, 0.9510565162951535312, 1.000000000000000000, 0.9510565162951535312, 1.000000000000000000, 0.9510565162951535312, 1.000000000000000000, 0.9510565162951535312, 1.000000000000000000, 0.9510565162951535312, 1.000000000000000000, 0.9510565162951535312, 1.000000000000000000, 0.9510565162951535312, 1.000000000000000000, 0.9510565162951535312, 1.000000000000000000, 0.9510565162951535312, 1.000000000000000000, 0.9510565162951535312, 1.000000000000000000, 0.9510565162951535312, 1.000000000000000000, 0.9510565162951535312, 1.000000000000000000, 0.9510565162951535312, 1.000000000000000000, 0.9510565162951535312, 1.000000000000000000, 0.9510565162951535312, 1.000000000000000000, 0.9510565162951535312, 1.000000000000000000, 0.9510565162951535312, 1.000000000000000000, 0.9510565162951535312, 1.000000000000000000, 0.9510565162951535312, 1.000000000000000000, 0.9510565162951535312, 1.000000000000000000, 0.9510565162951535312, 1.000000000000000000, 0.9510565162951535312, 1.000000000000000000, 0.9510565162951535312, 1.000000000000000000, 0.9510565162951535312, 1.000000000000000000, 0.9510565162951535312, 1.000000000000000000, 0.9510565162951535312, 1.000000000000000000, 0.9510565162951535312, 1.000000000000000000, 0.9510565162951535312, 1.000000000000000000, 0.9510565162951535312, 1.000000000000000000, 0.9510565162951535312, 1.000000000000000000, 0.9510565162951535312, 1.000000000000000000, 0.9510565162951535312, 1.000000000000000000, 0.9510565162951535312, 1.000000000000000000, 0.9510565162951535312, 1.000000000000000000, 0.9510565162951535312, 1.000000000000000000, 0.9510565162951535312, 1.000000000000000000, 0.9510565162951535312, 1.000000000000000000, 0.9510565162951535312, 1.000000000000000000, 0.9510565162951535312, 1.000000000000000000, 0.9510565162951535312, 1.000000000000000000, 0.9510565162951535312, 1.000000000000000000, 0.9510565162951535312, 1.000000000000000000, 0.9510565162951535312, 1.000000000000000000, 0.9510565162951535312, 1.000000000000000000, 0.9510565162951535312, 1.000000000000000000, 0.9510565162951535312, 1.000000000000000000, 0.9510565162951535312, 1.000000000000000000, 0.9510565162951535312, 1.000000000000000000, 0.9510565162951535312, 1.000000000000000000, 0.9510565162951535312, 1.000000000000000000, 0.9510565162951535312, 1.000000000000000000, 0.9510565162951535312, 1.000000000000000000, 0.9510565162951535312, 1.000000000000000000, 0.9510565162951535312, 1.000000000000000000, 0.9510565162951535312, 1.000000000000000000, 0.9510565162951535312, 1.000000000000000000, 0.9510565162951535312, 1.000000000000000000, 0.9510565162951535312, 1.000000000000000000, 0.9510565162951535312, 1.000000000000000000, 0.9510565162951535312, 1.000000000000000000, 0.9510565162951535312, 1.000000000000000000, 0.9510565162951535312, 1.000000000000000000, 0.9510565162951535312, 1.000000000000000000, 0.9510565162951535312, 1.000000000000000000, 0.9510565162951535312, 1.000000000000000000, 0.9510565162951535312, 1.000000000000000000, 0.9510565162951535312, 1.000000000000000000, 0.9510565162951535312, 1.000000000000000000, 0.9510565162951535312, 1.000000000000000000, 0.9510565162951535312, 1.000000000000000000, 0.9510565162951535312, 1.000000000000000000, 0.9510565162951535312, 1.000000000000000000, 0.9510565162951535312, 1.000000000000000000, 0.9510565162951535312, 1.000000000000000000, 0.9510565162951535312, 1.000000000000000000, 0.9510565162951535312, 1.000000000000000000, 0.9510565162951535312, 1.000000000000000000, 0.9510565162951535312, 1.000000000000000000, 0.9510565162951535312, 1.000000000000000000, 0.9510565162951535312, 1.000000000000000000, 0.9510565162951535312, 1.000000000000000000, 0.9510565162951535312, 1.000000000000000000, 0.9510565162951535312, 1.000000000000000000, 0.9510565162951535312, 1.000000000000000000, 0.9510565162951535312, 1.000000000000000000, 0.9510565162951535312, 1.000000000000000000, 0.9510565162951535312, 1.000000000000000000, 0.9510565162951535312, 1.000000000000000000, 0.9510565162951535312, 1.000000000000000000, 0.9510565162951535312, 1.000000000000000000, 0.9510565162951535312, 1.000000000000000000, 0.9510565162951535312, 1.000000000000000000, 0.9510565162951535312, 1.000000000000000000, 0.9836253951315760968, 0.9782074146920120006) ) ) 
 REPRESENTATION_ITEM ( '' )  SURFACE ( )  );
#14022 = CARTESIAN_POINT ( 'NONE',  ( 44.55648932407425633, 103.6104996726487428, 38.96596240072933170 ) ) ;
#14023 = CARTESIAN_POINT ( 'NONE',  ( 11.74529739132928619, 133.8467647624810581, -4.446451035385589279 ) ) ;
#14024 = DIRECTION ( 'NONE',  ( -1.000000000000000000, 0.000000000000000000, -1.233581138472395521E-15 ) ) ;
#14025 = EDGE_CURVE ( 'NONE', #17423, #5662, #7150, .T. ) ;
#14026 = CARTESIAN_POINT ( 'NONE',  ( -159.5594255724347761, -173.1891397928654897, 55.53486410454104316 ) ) ;
#14027 = CARTESIAN_POINT ( 'NONE',  ( 38.01140435219952707, 152.7844580088725763, 34.21067981925357060 ) ) ;
#14028 = DIRECTION ( 'NONE',  ( 0.000000000000000000, 0.000000000000000000, -1.000000000000000000 ) ) ;
#14029 = DIRECTION ( 'NONE',  ( 0.000000000000000000, 0.000000000000000000, 1.000000000000000000 ) ) ;
#14030 = ORIENTED_EDGE ( 'NONE', *, *, #11809, .F. ) ;
#14031 = CARTESIAN_POINT ( 'NONE',  ( 41.64333658814960870, 83.77977050742732956, 30.00020018409699318 ) ) ;
#14032 = CARTESIAN_POINT ( 'NONE',  ( -157.2955611005346270, -167.3438272943106995, 41.63779006702063867 ) ) ;
#14033 = CARTESIAN_POINT ( 'NONE',  ( 38.58424406990785371, 78.26518717409402370, 35.64915139335015937 ) ) ;
#14034 = CARTESIAN_POINT ( 'NONE',  ( 77.19215121279506775, 118.0176990621192203, -1.351406188750652992 ) ) ;
#14035 = CARTESIAN_POINT ( 'NONE',  ( -142.0420953463935803, -195.5084106276440536, 46.59394152635518793 ) ) ;
#14036 = ORIENTED_EDGE ( 'NONE', *, *, #3491, .F. ) ;
#14037 = CARTESIAN_POINT ( 'NONE',  ( -161.4692556286852891, -175.7130981290892748, 46.40781461928724383 ) ) ;
#14038 = DIRECTION ( 'NONE',  ( -1.000000000000000000, 0.000000000000000000, -4.622506457652816058E-16 ) ) ;
#14039 = CARTESIAN_POINT ( 'NONE',  ( 39.42975644700377558, 132.0797705074273267, 31.60846029578754468 ) ) ;
#14040 = CARTESIAN_POINT ( 'NONE',  ( 27.04509496028088478, 143.0549882411833380, 11.23409068567602098 ) ) ;
#14041 = ORIENTED_EDGE ( 'NONE', *, *, #11706, .F. ) ;
#14042 = EDGE_CURVE ( 'NONE', #17319, #7289, #394, .T. ) ;
#14043 = DIRECTION ( 'NONE',  ( 1.000000000000000000, 0.000000000000000000, 0.000000000000000000 ) ) ;
#14044 = ORIENTED_EDGE ( 'NONE', *, *, #3466, .T. ) ;
#14045 = CARTESIAN_POINT ( 'NONE',  ( 40.27526882409969033, 137.9297705074273210, 30.44471234641811819 ) ) ;
#14046 = EDGE_CURVE ( 'NONE', #7555, #17533, #8667, .T. ) ;
#14047 = AXIS2_PLACEMENT_3D ( 'NONE', #21716, #1429, #9922 ) ;
#14048 = AXIS2_PLACEMENT_3D ( 'NONE', #14748, #18162, #6489 ) ;
#14049 = CARTESIAN_POINT ( 'NONE',  ( 43.01140435219951996, 10.71049967264875491, 39.21067981925356349 ) ) ;
#14050 = CARTESIAN_POINT ( 'NONE',  ( 48.01140435219951996, 121.2844580088725763, 34.21067981925357060 ) ) ;
#14051 = CARTESIAN_POINT ( 'NONE',  ( -149.8854112254399524, -194.3899795514095388, 39.65701158161630246 ) ) ;
#14052 = EDGE_CURVE ( 'NONE', #811, #13269, #10428, .T. ) ;
#14053 = CARTESIAN_POINT ( 'NONE',  ( 45.74753988029933538, 97.16518717409398675, 37.97664729208901946 ) ) ;
#14054 = CARTESIAN_POINT ( 'NONE',  ( 48.01140435219951996, 133.2844580088726048, 34.21067981925357060 ) ) ;
#14055 = CARTESIAN_POINT ( 'NONE',  ( 18.67254549292281141, -61.68114226949890622, 20.00000000000000355 ) ) ;
#14056 = CARTESIAN_POINT ( 'NONE',  ( -151.4692556286852891, -156.8130981290892692, 60.17163382399899518 ) ) ;
#14057 = CARTESIAN_POINT ( 'NONE',  ( 38.96631938032478359, 129.0844580088725877, 37.14960608071593384 ) ) ;
#14058 = CARTESIAN_POINT ( 'NONE',  ( 38.58424406990784661, 111.5297705074273154, 35.64915139335016647 ) ) ;
#14059 = CARTESIAN_POINT ( 'NONE',  ( 46.21245884545565019, 91.80782910428004584, 13.29499484581607582 ) ) ;
#14060 = CARTESIAN_POINT ( 'NONE',  ( -157.2955611005346270, -190.4438272943107506, 57.67623309621198047 ) ) ;
#14061 = CARTESIAN_POINT ( 'NONE',  ( 43.01140435219951286, 105.8651871740939896, 38.86567161673127657 ) ) ;
#14062 = DIRECTION ( 'NONE',  ( -0.2803088796301151375, 0.9599098561846886035, 0.000000000000000000 ) ) ;
#14063 = ORIENTED_EDGE ( 'NONE', *, *, #7909, .T. ) ;
#14064 = CARTESIAN_POINT ( 'NONE',  ( 43.80332655382220963, 157.9575765865523351, 29.21067981925357060 ) ) ;
#14065 = CARTESIAN_POINT ( 'NONE',  ( 23.63511980923729183, 148.0372221624750466, 11.16864677238829984 ) ) ;
#14066 = CARTESIAN_POINT ( 'NONE',  ( 65.77248029998415291, 103.2585056976580091, 13.37079068582577435 ) ) ;
#14067 = LINE ( 'NONE', #13851, #9002 ) ;
#14068 = CARTESIAN_POINT ( 'NONE',  ( 47.43856463449117911, 77.02977050742731535, 32.77220824515697473 ) ) ;
#14069 = ORIENTED_EDGE ( 'NONE', *, *, #16764, .T. ) ;
#14070 = ADVANCED_FACE ( 'NONE', ( #1724 ), #13829, .F. ) ;
#14071 = CARTESIAN_POINT ( 'NONE',  ( 46.10157429594899270, 60.83445800887256638, 38.46393386101376421 ) ) ;
#14072 = CARTESIAN_POINT ( 'NONE',  ( -141.4692556286852891, -165.2130981290893033, 52.90620854394536821 ) ) ;
#14073 = CARTESIAN_POINT ( 'NONE',  ( 38.01140435219951996, 117.5604996726487315, 32.58608133808903773 ) ) ;
#14075 = CARTESIAN_POINT ( 'NONE',  ( 66.55041322599720388, 95.16028120083096553, -6.513516925475251185 ) ) ;
#14074 = CARTESIAN_POINT ( 'NONE',  ( 39.42975644700377558, 81.41518717409400097, 36.81289934271958941 ) ) ;
#14076 = CARTESIAN_POINT ( 'NONE',  ( -142.0420953463935803, -177.2438272943107336, 46.59394152635518083 ) ) ;
#14077 = CARTESIAN_POINT ( 'NONE',  ( 44.55648932407425633, 113.8104996726487457, 29.45539723777780239 ) ) ;
#14078 = CARTESIAN_POINT ( 'NONE',  ( -154.5594255724347761, -189.9630981290893317, 59.16757674456785310 ) ) ;
#14079 = VECTOR ( 'NONE', #9718, 1000.000000000000114 ) ;
#14080 = CARTESIAN_POINT ( 'NONE',  ( 46.10157429594899270, 67.76049967264873430, 38.46393386101375711 ) ) ;
#14081 = CARTESIAN_POINT ( 'NONE',  ( -149.8854112254399809, -163.6622583705451746, 59.65701158161633089 ) ) ;
#14082 = CARTESIAN_POINT ( 'NONE',  ( 43.01140435219951286, 140.6297705074273097, 29.55568802177586463 ) ) ;
#14083 = EDGE_CURVE ( 'NONE', #20743, #16099, #9401, .T. ) ;
#14084 = CARTESIAN_POINT ( 'NONE',  ( 45.74753988029933538, 104.3297705074272983, 30.44471234641811819 ) ) ;
#14085 = CARTESIAN_POINT ( 'NONE',  ( 39.42975644700377558, 132.4151871740940010, 36.81289934271958941 ) ) ;
#14086 = CARTESIAN_POINT ( 'NONE',  ( -148.5561028927606344, -155.7938272943107449, 40.69124936498395328 ) ) ;
#14087 = CARTESIAN_POINT ( 'NONE',  ( -159.0959885057557983, -160.8584106276440480, 55.19815736654470584 ) ) ;
#14088 = CARTESIAN_POINT ( 'NONE',  ( -27.64582385433943656, -34.13255853780189142, 5.000000000000018652 ) ) ;
#14089 = DIRECTION ( 'NONE',  ( 0.000000000000000000, 1.000000000000000000, 0.000000000000000000 ) ) ;
#14090 = CARTESIAN_POINT ( 'NONE',  ( 66.29928749942908439, 103.8601778506706239, 12.34270352495849110 ) ) ;
#14091 = DIRECTION ( 'NONE',  ( 0.000000000000000000, 1.000000000000000000, 0.000000000000000000 ) ) ;
#14092 = CARTESIAN_POINT ( 'NONE',  ( 44.37947211624943833, 116.2151871740940123, 30.00020018409699318 ) ) ;
#14093 = EDGE_CURVE ( 'NONE', #14386, #13487, #20136, .T. ) ;
#14094 = ORIENTED_EDGE ( 'NONE', *, *, #7191, .F. ) ;
#14095 =( GEOMETRIC_REPRESENTATION_CONTEXT ( 3 ) GLOBAL_UNCERTAINTY_ASSIGNED_CONTEXT ( ( #10628 ) ) GLOBAL_UNIT_ASSIGNED_CONTEXT ( ( #12225, #2621, #7716 ) ) REPRESENTATION_CONTEXT ( 'NONE', 'WORKASPACE' ) );
#14096 = CARTESIAN_POINT ( 'NONE',  ( -161.4692556286852891, -160.7130981290893033, 46.40781461928724383 ) ) ;
#14097 = ORIENTED_EDGE ( 'NONE', *, *, #19040, .F. ) ;
#14098 = CARTESIAN_POINT ( 'NONE',  ( 39.92123440845004723, 92.33445800887255928, 29.95742577749337343 ) ) ;
#14099 = CARTESIAN_POINT ( 'NONE',  ( 39.42975644700377558, 150.6797705074273210, 36.81289934271958941 ) ) ;
#14100 = CARTESIAN_POINT ( 'NONE',  ( 46.10157429594899270, 157.7604996726487343, 38.46393386101376421 ) ) ;
#14102 = CARTESIAN_POINT ( 'NONE',  ( 22.01597290215339697, 101.2010103422484519, -4.648787059867797389 ) ) ;
#14101 = CARTESIAN_POINT ( 'NONE',  ( 43.01140435219951286, 105.8651871740939754, 38.86567161673127657 ) ) ;
#14103 = CARTESIAN_POINT ( 'NONE',  ( 47.05648932407426344, 74.51049967264873430, 31.27175355779120025 ) ) ;
#14105 = CARTESIAN_POINT ( 'NONE',  ( -32.30114424549768870, -19.06233958201669410, -25.00000000000000000 ) ) ;
#14104 = DIRECTION ( 'NONE',  ( 0.000000000000000000, 1.000000000000000000, 0.000000000000000000 ) ) ;
#14106 = CARTESIAN_POINT ( 'NONE',  ( -154.5594255724347761, -191.1630981290893203, 40.14644641866476604 ) ) ;
#14107 = CARTESIAN_POINT ( 'NONE',  ( 46.59305225739526435, 70.31518717409400665, 36.81289934271958941 ) ) ;
#14108 = CARTESIAN_POINT ( 'NONE',  ( 159.0505745212445561, 203.5296818892961994, 34.00000000000001421 ) ) ;
#14109 = CARTESIAN_POINT ( 'NONE',  ( -151.4692556286852891, -178.1438272943106824, 59.56931450028537967 ) ) ;
#14110 = CARTESIAN_POINT ( 'NONE',  ( 45.51148226160370314, 59.71123016864974176, 29.88059778228138086 ) ) ;
#14111 = ORIENTED_EDGE ( 'NONE', *, *, #3646, .T. ) ;
#14112 = CARTESIAN_POINT ( 'NONE',  ( -142.0420953463936087, -180.6584106276440309, 49.65701158161630957 ) ) ;
#14113 = CARTESIAN_POINT ( 'NONE',  ( 51.59368247783319816, 153.1301807948854616, 10.12058642595840929 ) ) ;
#14114 = EDGE_CURVE ( 'NONE', #175, #12379, #15050, .T. ) ;
#14115 = ORIENTED_EDGE ( 'NONE', *, *, #7870, .T. ) ;
#14116 = CARTESIAN_POINT ( 'NONE',  ( 39.42975644700377558, 140.8151871740940067, 31.60846029578754468 ) ) ;
#14117 = CARTESIAN_POINT ( 'NONE',  ( 38.58424406990785371, 108.5297705074273011, 35.64915139335015937 ) ) ;
#14118 = ORIENTED_EDGE ( 'NONE', *, *, #17825, .T. ) ;
#14119 = ORIENTED_EDGE ( 'NONE', *, *, #10481, .T. ) ;
#14120 = CARTESIAN_POINT ( 'NONE',  ( 69.49396330798431620, 129.5978393632817927, 5.275421687385184910 ) ) ;
#14121 = ORIENTED_EDGE ( 'NONE', *, *, #882, .T. ) ;
#14122 = CARTESIAN_POINT ( 'NONE',  ( 38.01140435219951996, 116.9344580088725820, 35.83527830041810347 ) ) ;
#14123 = EDGE_CURVE ( 'NONE', #19018, #17658, #3595, .T. ) ;
#14124 = DIRECTION ( 'NONE',  ( 0.000000000000000000, 0.000000000000000000, 1.000000000000000000 ) ) ;
#14125 = CARTESIAN_POINT ( 'NONE',  ( 38.58424406990784661, 143.9651871740940123, 32.77220824515698183 ) ) ;
#14126 = CARTESIAN_POINT ( 'NONE',  ( 41.46631938032478359, 105.1104996726487428, 29.45539723777780239 ) ) ;
#14127 = CARTESIAN_POINT ( 'NONE',  ( 69.71972837475884432, 98.49221204361529658, -7.660766391518695428 ) ) ;
#14128 = PLANE ( 'NONE',  #8964 ) ;
#14129 = CARTESIAN_POINT ( 'NONE',  ( -145.2889157411863721, -172.4391397928654612, 58.16351966513671812 ) ) ;
#14130 = CARTESIAN_POINT ( 'NONE',  ( 43.80332655382220963, 158.8836182503284533, 29.21067981925357060 ) ) ;
#14131 = UNCERTAINTY_MEASURE_WITH_UNIT (LENGTH_MEASURE( 1.000000000000000082E-05 ), #2724, 'distance_accuracy_value', 'NONE');
#14132 = CARTESIAN_POINT ( 'NONE',  ( 42.21948215057684450, 143.1113394311928460, 29.21067981925356705 ) ) ;
#14133 = AXIS2_PLACEMENT_3D ( 'NONE', #16171, #12983, #21475 ) ;
#14134 = CARTESIAN_POINT ( 'NONE',  ( 46.10157429594899270, 105.8344580088725735, 38.46393386101375711 ) ) ;
#14135 = VECTOR ( 'NONE', #7339, 1000.000000000000114 ) ;
#14136 = EDGE_LOOP ( 'NONE', ( #10850, #8802, #18474, #14447 ) ) ;
#14137 = CARTESIAN_POINT ( 'NONE',  ( 46.59305225739526435, 86.17977050742732104, 31.60846029578754468 ) ) ;
#14138 = CARTESIAN_POINT ( 'NONE',  ( -151.4692556286852891, -166.1438272943107393, 59.56931450028537967 ) ) ;
#14139 = CARTESIAN_POINT ( 'NONE',  ( 41.64333658814960870, 66.71518717409399812, 38.42115945441014446 ) ) ;
#14140 = CARTESIAN_POINT ( 'NONE',  ( 74.85601106972485752, 107.3429126181175661, -0.9942341299615756745 ) ) ;
#14141 = CARTESIAN_POINT ( 'NONE',  ( -142.0420953463935803, -192.5084106276439968, 46.59394152635518793 ) ) ;
#14142 = VECTOR ( 'NONE', #4026, 1000.000000000000000 ) ;
#14143 = ORIENTED_EDGE ( 'NONE', *, *, #4945, .F. ) ;
#14144 = CARTESIAN_POINT ( 'NONE',  ( 129.2454342010813662, 193.1635054290503319, -44.99999999999997158 ) ) ;
#14145 = CARTESIAN_POINT ( 'NONE',  ( 38.01140435219952707, 104.7844580088725763, 34.21067981925357060 ) ) ;
#14146 = CARTESIAN_POINT ( 'NONE',  ( 45.74753988029934249, 130.4297705074273210, 37.97664729208901235 ) ) ;
#14147 = CARTESIAN_POINT ( 'NONE',  ( 27.89715912807487186, 143.6191053679247602, 4.279900468622926724 ) ) ;
#14148 = ORIENTED_EDGE ( 'NONE', *, *, #12306, .T. ) ;
#14149 =( BOUNDED_CURVE ( )  B_SPLINE_CURVE ( 2, ( #6995, #12145, #20117, #2022, #18879, #13379, #5328, #8754, #20221, #8541, #3787, #11831, #15471 ),
 .UNSPECIFIED., .F., .F. ) 
 B_SPLINE_CURVE_WITH_KNOTS ( ( 3, 2, 2, 2, 2, 2, 3 ),
 ( 0.3161764705882352811, 0.3176470588235293935, 0.3205882352941176738, 0.3235294117647058987, 0.3264705882352941235, 0.3294117647058823484, 0.3308823529411764608 ),
 .UNSPECIFIED. ) 
 CURVE ( )  GEOMETRIC_REPRESENTATION_ITEM ( )  RATIONAL_B_SPLINE_CURVE ( ( 0.9755282581475768211, 0.9755282581475768211, 1.000000000000000000, 0.9510565162951535312, 1.000000000000000000, 0.9510565162951535312, 1.000000000000000000, 0.9510565162951535312, 1.000000000000000000, 0.9510565162951535312, 1.000000000000000000, 0.9755282581475768211, 0.9755282581475768211 ) ) 
 REPRESENTATION_ITEM ( '' )  );
#14150 = ORIENTED_EDGE ( 'NONE', *, *, #13655, .F. ) ;
#14151 = CARTESIAN_POINT ( 'NONE',  ( 40.27526882409969033, 126.8297705074273409, 37.97664729208901946 ) ) ;
#14152 = LINE ( 'NONE', #9212, #6978 ) ;
#14153 = VECTOR ( 'NONE', #20554, 1000.000000000000000 ) ;
#14154 = CARTESIAN_POINT ( 'NONE',  ( 44.55648932407425633, 154.6104996726487570, 38.96596240072933170 ) ) ;
#14155 = EDGE_CURVE ( 'NONE', #17073, #1468, #13601, .T. ) ;
#14156 = CARTESIAN_POINT ( 'NONE',  ( -151.4692556286852607, -168.8130981290893260, 59.65701158161632378 ) ) ;
#14157 = CARTESIAN_POINT ( 'NONE',  ( 47.05648932407426344, 120.9844580088725934, 37.14960608071593384 ) ) ;
#14158 = LINE ( 'NONE', #19339, #13005 ) ;
#14159 = EDGE_CURVE ( 'NONE', #20087, #1303, #10322, .T. ) ;
#14160 = CARTESIAN_POINT ( 'NONE',  ( 47.43856463449117200, 97.46518717409399812, 35.64915139335016647 ) ) ;
#14161 = CARTESIAN_POINT ( 'NONE',  ( 46.10157429594899270, 73.76049967264873430, 38.46393386101375711 ) ) ;
#14162 = CARTESIAN_POINT ( 'NONE',  ( 44.55648932407425633, 125.8104996726487315, 29.45539723777780239 ) ) ;
#14163 = CARTESIAN_POINT ( 'NONE',  ( -159.5594255724347761, -160.2630981290893146, 55.53486410454104316 ) ) ;
#14164 = APPLICATION_PROTOCOL_DEFINITION ( 'draft international standard', 'automotive_design', 1998, #289 ) ;
#14165 = CARTESIAN_POINT ( 'NONE',  ( 48.01140435219951996, 109.4344580088725820, 32.58608133808903773 ) ) ;
#14166 = CARTESIAN_POINT ( 'NONE',  ( 39.92123440845004723, 135.2344580088725650, 38.46393386101376421 ) ) ;
#14167 = CARTESIAN_POINT ( 'NONE',  ( 46.59305225739526435, 112.5797705074273125, 36.81289934271958941 ) ) ;
#14168 = CARTESIAN_POINT ( 'NONE',  ( 17.32321720400341292, 131.7349665092470730, 8.652027877775747555 ) ) ;
#14169 = CARTESIAN_POINT ( 'NONE',  ( 101.6431471920911207, 239.2647937927896464, -5.999999999999976019 ) ) ;
#14170 = CARTESIAN_POINT ( 'NONE',  ( 47.43856463449117911, 97.76518717409398107, 32.77220824515697473 ) ) ;
#14171 = CARTESIAN_POINT ( 'NONE',  ( 77.34521997529867576, 314.8592298662555322, -4.000000000000004441 ) ) ;
#14172 = ORIENTED_EDGE ( 'NONE', *, *, #5643, .T. ) ;
#14173 = CARTESIAN_POINT ( 'NONE',  ( 48.01140435219951996, 157.2844580088725763, 34.21067981925357060 ) ) ;
#14174 = CARTESIAN_POINT ( 'NONE',  ( 50.33192209904863290, 153.3481575868430014, -9.922832680162505525 ) ) ;
#14175 = CARTESIAN_POINT ( 'NONE',  ( 51.84853669763433004, 93.12814091139611605, 7.061107544354192633 ) ) ;
#14176 = DIRECTION ( 'NONE',  ( 0.000000000000000000, 1.000000000000000000, 0.000000000000000000 ) ) ;
#14177 = CARTESIAN_POINT ( 'NONE',  ( 39.42975644700377558, 72.07977050742732672, 31.60846029578754468 ) ) ;
#14178 = EDGE_LOOP ( 'NONE', ( #6630, #2440, #16753, #3558, #17616, #13480 ) ) ;
#14179 = ORIENTED_EDGE ( 'NONE', *, *, #5560, .T. ) ;
#14180 = CARTESIAN_POINT ( 'NONE',  ( -149.8854112254399809, -164.3899795514095672, 39.65701158161628825 ) ) ;
#14181 = CARTESIAN_POINT ( 'NONE',  ( 48.01140435219951996, 125.0604996726487741, 35.83527830041810347 ) ) ;
#14183 = CARTESIAN_POINT ( 'NONE',  ( 14.82542406694137860, 100.6198891296320994, 2.415082931867933880 ) ) ;
#14182 = CARTESIAN_POINT ( 'NONE',  ( 43.01140435219951286, 77.36518717409400381, 29.55568802177586463 ) ) ;
#14184 = CARTESIAN_POINT ( 'NONE',  ( -151.4692556286852891, -175.1438272943107393, 59.56931450028537256 ) ) ;
#14185 = DIRECTION ( 'NONE',  ( 0.9385982292947090411, 0.3450121214752271959, -1.756657601269562932E-16 ) ) ;
#14186 = CARTESIAN_POINT ( 'NONE',  ( -151.4692556286852891, -186.8130981290893260, 60.17163382399899518 ) ) ;
#14187 =( NAMED_UNIT ( * ) SI_UNIT ( $, .STERADIAN. ) SOLID_ANGLE_UNIT ( ) );
#14188 = CARTESIAN_POINT ( 'NONE',  ( 148.6725454929228079, -61.68114226949890622, 20.00000000000001776 ) ) ;
#14189 = CARTESIAN_POINT ( 'NONE',  ( 41.46631938032478359, 149.1844580088725820, 29.45539723777780239 ) ) ;
#14190 = CARTESIAN_POINT ( 'NONE',  ( 43.01140435219951286, 143.6297705074272812, 29.55568802177586463 ) ) ;
#14191 = CARTESIAN_POINT ( 'NONE',  ( 69.47322557110069852, 98.06143112153284846, 5.358778726746561638 ) ) ;
#14192 = CARTESIAN_POINT ( 'NONE',  ( 47.43856463449118621, 136.6151871740940180, 34.21067981925357060 ) ) ;
#14193 = CARTESIAN_POINT ( 'NONE',  ( 132.3486983259487886, 110.2203079035326851, -35.00000000000000000 ) ) ;
#14194 = CARTESIAN_POINT ( 'NONE',  ( -157.2955611005345986, -166.7084106276440423, 57.67623309621197336 ) ) ;
#14195 = ADVANCED_FACE ( 'NONE', ( #12502 ), #603, .T. ) ;
#14196 = CARTESIAN_POINT ( 'NONE',  ( 45.22505347682923826, 59.38050100342834270, 30.37668637662395099 ) ) ;
#14197 = DIRECTION ( 'NONE',  ( -0.3428981916074304581, 0.9393725726208712601, 0.000000000000000000 ) ) ;
#14198 = EDGE_CURVE ( 'NONE', #10505, #15773, #2889, .T. ) ;
#14199 = CARTESIAN_POINT ( 'NONE',  ( 62.80402591640378773, 99.70611228127967252, 5.556743651330835476 ) ) ;
#14200 = DIRECTION ( 'NONE',  ( 0.000000000000000000, -1.000000000000000000, 0.000000000000000000 ) ) ;
#14201 = CARTESIAN_POINT ( 'NONE',  ( 46.59305225739526435, 103.9151871740940152, 31.60846029578754468 ) ) ;
#14202 = ORIENTED_EDGE ( 'NONE', *, *, #16946, .F. ) ;
#14203 = DIRECTION ( 'NONE',  ( -0.4999999999999993894, 0.000000000000000000, 0.8660254037844389297 ) ) ;
#14204 = ORIENTED_EDGE ( 'NONE', *, *, #4893, .T. ) ;
#14205 = CARTESIAN_POINT ( 'NONE',  ( 41.46631938032478359, 93.38445800887258486, 38.96596240072933170 ) ) ;
#14206 = CARTESIAN_POINT ( 'NONE',  ( 38.01140435219951996, 150.5604996726487741, 32.58608133808903773 ) ) ;
#14208 = CARTESIAN_POINT ( 'NONE',  ( 15.04800518778627882, 122.8738276488686694, -10.72018599084894319 ) ) ;
#14207 = CARTESIAN_POINT ( 'NONE',  ( 43.01140435219951286, 108.8651871740939896, 38.86567161673127657 ) ) ;
#14209 = CARTESIAN_POINT ( 'NONE',  ( 38.01140435219952707, 60.71049967264874425, 34.21067981925357060 ) ) ;
#14211 = CYLINDRICAL_SURFACE ( 'NONE', #17086, 15.56217413224114310 ) ;
#14210 = CARTESIAN_POINT ( 'NONE',  ( 157.5268905834513475, 193.0332408774651185, 14.00000000000001776 ) ) ;
#14212 = ADVANCED_FACE ( 'NONE', ( #19016 ), #7343, .T. ) ;
#14213 = CARTESIAN_POINT ( 'NONE',  ( 46.10157429594899270, 79.73445800887257917, 29.95742577749336988 ) ) ;
#14214 = DIRECTION ( 'NONE',  ( 1.000000000000000000, 0.000000000000000000, 0.000000000000000000 ) ) ;
#14215 = CARTESIAN_POINT ( 'NONE',  ( 47.43856463449117200, 67.76518717409399528, 32.77220824515698183 ) ) ;
#14216 = CARTESIAN_POINT ( 'NONE',  ( 71.14040157825178312, 139.4183699182763974, -9.089337262093875935 ) ) ;
#14217 = CARTESIAN_POINT ( 'NONE',  ( 48.01140435219951996, 104.2104996726487371, 34.21067981925357060 ) ) ;
#14218 = CARTESIAN_POINT ( 'NONE',  ( -159.0959885057557983, -175.5938272943107279, 55.19815736654470584 ) ) ;
#14219 = CARTESIAN_POINT ( 'NONE',  ( -143.8425227516148084, -192.3584106276440480, 44.11586579668791330 ) ) ;
#14220 = VERTEX_POINT ( 'NONE', #10644 ) ;
#14221 = CARTESIAN_POINT ( 'NONE',  ( -142.0420953463935803, -177.5084106276440536, 46.59394152635518793 ) ) ;
#14222 = CARTESIAN_POINT ( 'NONE',  ( 8.843693174888816344, 123.0768258502195067, 1.191984145255910787 ) ) ;
#14223 = CARTESIAN_POINT ( 'NONE',  ( 43.01140435219951996, 10.71049967264875491, 34.21067981925357060 ) ) ;
#14224 = CARTESIAN_POINT ( 'NONE',  ( 43.01140435219951286, 140.3651871740940180, 29.55568802177586463 ) ) ;
#14225 = CARTESIAN_POINT ( 'NONE',  ( 45.74753988029934249, 107.3297705074272983, 30.44471234641812174 ) ) ;
#14226 = ORIENTED_EDGE ( 'NONE', *, *, #11753, .F. ) ;
#14227 = ORIENTED_EDGE ( 'NONE', *, *, #12984, .T. ) ;
#14228 = CARTESIAN_POINT ( 'NONE',  ( 46.56541826512206228, 91.93282113015048651, 0.2755065429245392439 ) ) ;
#14229 = ORIENTED_EDGE ( 'NONE', *, *, #11333, .F. ) ;
#14230 = CARTESIAN_POINT ( 'NONE',  ( 38.01140435219952707, 113.7844580088725763, 34.21067981925357060 ) ) ;
#14231 = AXIS2_PLACEMENT_3D ( 'NONE', #3786, #11940, #10405 ) ;
#14232 = CARTESIAN_POINT ( 'NONE',  ( 147.5268905834513475, 193.0332408774651185, -50.99999999999998579 ) ) ;
#14233 = CARTESIAN_POINT ( 'NONE',  ( 46.59305225739526435, 79.57977050742731251, 36.81289934271958941 ) ) ;
#14234 = CARTESIAN_POINT ( 'NONE',  ( 43.01140435219951286, 132.8651871740940180, 38.86567161673127657 ) ) ;
#14235 = CARTESIAN_POINT ( 'NONE',  ( 46.10157429594899270, 98.66049967264872578, 29.95742577749337343 ) ) ;
#14236 = CARTESIAN_POINT ( 'NONE',  ( 70.62757080055673953, 99.67629488849819097, 13.29148015538516425 ) ) ;
#14237 = ADVANCED_FACE ( 'NONE', ( #5880 ), #5668, .T. ) ;
#14238 = CARTESIAN_POINT ( 'NONE',  ( 48.01140435219951996, 119.3604996726487570, 32.58608133808903773 ) ) ;
#14239 = CARTESIAN_POINT ( 'NONE',  ( -159.5594255724347761, -158.1891397928654612, 55.53486410454104316 ) ) ;
#14240 = CARTESIAN_POINT ( 'NONE',  ( 38.01140435219952707, 152.6344580088725706, 32.58608133808903773 ) ) ;
#14241 = CARTESIAN_POINT ( 'NONE',  ( 47.05648932407426344, 106.5844580088725877, 31.27175355779120025 ) ) ;
#14242 = ORIENTED_EDGE ( 'NONE', *, *, #2399, .T. ) ;
#14243 = CARTESIAN_POINT ( 'NONE',  ( 38.58424406990784661, 84.22977050742730398, 32.77220824515698183 ) ) ;
#14244 = CARTESIAN_POINT ( 'NONE',  ( 17.73005198514846725, 142.9879744078657779, -4.089424278207452801 ) ) ;
#14245 = DIRECTION ( 'NONE',  ( -1.000000000000000000, 0.000000000000000000, 0.000000000000000000 ) ) ;
#14246 = VERTEX_POINT ( 'NONE', #7554 ) ;
#14247 = CARTESIAN_POINT ( 'NONE',  ( 38.01140435219952707, 104.6344580088725564, 32.58608133808903773 ) ) ;
#14248 = CARTESIAN_POINT ( 'NONE',  ( 40.27526882409969744, 131.9297705074273210, 30.44471234641812174 ) ) ;
#14249 = CARTESIAN_POINT ( 'NONE',  ( 10.62509257988331335, 109.0622927966340967, -11.27555259023744405 ) ) ;
#14250 = EDGE_LOOP ( 'NONE', ( #18300, #18874, #1987, #9851 ) ) ;
#14251 = CIRCLE ( 'NONE', #8645, 7.500000000000000000 ) ;
#14252 = CARTESIAN_POINT ( 'NONE',  ( 43.01140435219951286, 74.03445800887257633, 29.21067981925356705 ) ) ;
#14253 = ORIENTED_EDGE ( 'NONE', *, *, #5368, .T. ) ;
#14254 = CARTESIAN_POINT ( 'NONE',  ( 47.43856463449118621, 130.8797705074273381, 34.21067981925357060 ) ) ;
#14255 = DIRECTION ( 'NONE',  ( 0.000000000000000000, 0.000000000000000000, 1.000000000000000000 ) ) ;
#14256 = CARTESIAN_POINT ( 'NONE',  ( 47.43856463449117200, 89.02977050742731535, 32.77220824515698183 ) ) ;
#14257 = EDGE_CURVE ( 'NONE', #20193, #12027, #12611, .T. ) ;
#14258 = CARTESIAN_POINT ( 'NONE',  ( 43.01140435219951286, 128.9604996726487229, 29.21067981925356705 ) ) ;
#14259 = DIRECTION ( 'NONE',  ( 0.000000000000000000, 0.000000000000000000, -1.000000000000000000 ) ) ;
#14260 = CARTESIAN_POINT ( 'NONE',  ( -141.4692556286852891, -192.9891397928654726, 49.65701158161630957 ) ) ;
#14261 = CARTESIAN_POINT ( 'NONE',  ( 41.64333658814960870, 84.71518717409399812, 38.42115945441014446 ) ) ;
#14262 = LINE ( 'NONE', #4138, #261 ) ;
#14263 = CARTESIAN_POINT ( 'NONE',  ( 46.10157429594899270, 124.7604996726487343, 38.46393386101375711 ) ) ;
#14264 = CARTESIAN_POINT ( 'NONE',  ( -143.3790856849358306, -156.3630981290893089, 55.53486410454105027 ) ) ;
#14265 =( NAMED_UNIT ( * ) PLANE_ANGLE_UNIT ( ) SI_UNIT ( $, .RADIAN. ) );
#14266 = AXIS2_PLACEMENT_3D ( 'NONE', #5678, #21116, #2263 ) ;
#14267 = CARTESIAN_POINT ( 'NONE',  ( 38.01140435219952707, 131.9344580088725820, 35.83527830041809636 ) ) ;
#14268 = CARTESIAN_POINT ( 'NONE',  ( 48.01140435219951996, 133.1344580088725991, 35.83527830041810347 ) ) ;
#14269 = CARTESIAN_POINT ( 'NONE',  ( 40.27526882409969033, 117.8297705074273267, 37.97664729208901946 ) ) ;
#14270 = CARTESIAN_POINT ( 'NONE',  ( 41.03523200113699687, 148.1191603456353789, 9.842457937073838536 ) ) ;
#14271 = CARTESIAN_POINT ( 'NONE',  ( -142.0420953463935803, -189.2438272943107336, 46.59394152635518793 ) ) ;
#14272 = CARTESIAN_POINT ( 'NONE',  ( 40.27526882409969744, 93.56518717409397823, 37.97664729208901235 ) ) ;
#14273 = CARTESIAN_POINT ( 'NONE',  ( 67.34521997529867576, 314.8592298662555322, 272.0939500981630204 ) ) ;
#14274 = ORIENTED_EDGE ( 'NONE', *, *, #5860, .F. ) ;
#14275 = CARTESIAN_POINT ( 'NONE',  ( -39.76538861119684753, -7.722638610254815461, 4.000000000000021316 ) ) ;
#14276 = CARTESIAN_POINT ( 'NONE',  ( 69.83118287335672392, 141.1824132108841638, 4.838974892866481525 ) ) ;
#14277 =( BOUNDED_CURVE ( )  B_SPLINE_CURVE ( 2, ( #10229, #513, #11978, #18602, #17253, #15404, #1737, #10118, #10337, #12083, #5261, #186, #3826 ),
 .UNSPECIFIED., .F., .F. ) 
 B_SPLINE_CURVE_WITH_KNOTS ( ( 3, 2, 2, 2, 2, 2, 3 ),
 ( 0.1691176470588235115, 0.1705882352941176516, 0.1735294117647058765, 0.1764705882352941291, 0.1794117647058823539, 0.1823529411764705788, 0.1838235294117646912 ),
 .UNSPECIFIED. ) 
 CURVE ( )  GEOMETRIC_REPRESENTATION_ITEM ( )  RATIONAL_B_SPLINE_CURVE ( ( 0.9755282581475765991, 0.9755282581475764880, 1.000000000000000000, 0.9510565162951535312, 1.000000000000000000, 0.9510565162951535312, 1.000000000000000000, 0.9510565162951535312, 1.000000000000000000, 0.9510565162951535312, 1.000000000000000000, 0.9755282581475769321, 0.9755282581475765991 ) ) 
 REPRESENTATION_ITEM ( '' )  );
#14278 = CARTESIAN_POINT ( 'NONE',  ( 70.04389262751028866, 127.6510855156269599, -14.64878692017946626 ) ) ;
#14279 = CARTESIAN_POINT ( 'NONE',  ( -143.3790856849358306, -169.2891397928654840, 55.53486410454105027 ) ) ;
#14280 =( GEOMETRIC_REPRESENTATION_CONTEXT ( 3 ) GLOBAL_UNCERTAINTY_ASSIGNED_CONTEXT ( ( #5758 ) ) GLOBAL_UNIT_ASSIGNED_CONTEXT ( ( #9575, #14411, #863 ) ) REPRESENTATION_CONTEXT ( 'NONE', 'WORKASPACE' ) );
#14281 = CARTESIAN_POINT ( 'NONE',  ( 41.64333658814960870, 75.97977050742731819, 38.42115945441014446 ) ) ;
#14282 = ORIENTED_EDGE ( 'NONE', *, *, #5172, .F. ) ;
#14283 = EDGE_LOOP ( 'NONE', ( #11117, #16852, #11735, #9481 ) ) ;
#14284 = CARTESIAN_POINT ( 'NONE',  ( 44.37947211624943833, 155.4797705074273324, 30.00020018409699318 ) ) ;
#14285 = AXIS2_PLACEMENT_3D ( 'NONE', #6201, #17988, #21102 ) ;
#14286 = LINE ( 'NONE', #12532, #2790 ) ;
#14287 = CARTESIAN_POINT ( 'NONE',  ( 47.05648932407426344, 118.9104996726487400, 37.14960608071593384 ) ) ;
#14289 = CARTESIAN_POINT ( 'NONE',  ( 75.66441332552922461, 109.8968089748874064, -0.08503035249486777525 ) ) ;
#14288 = CARTESIAN_POINT ( 'NONE',  ( 46.59305225739526435, 76.31518717409399244, 36.81289934271958941 ) ) ;
#14290 = CARTESIAN_POINT ( 'NONE',  ( -160.8964159109769696, -172.8938272943107393, 49.65701158161630957 ) ) ;
#14291 = CARTESIAN_POINT ( 'NONE',  ( 74.27779736592162863, 105.9683817680885056, 13.05343286460986363 ) ) ;
#14292 = CARTESIAN_POINT ( 'NONE',  ( -145.2889157411863721, -183.5130981290892578, 58.16351966513671812 ) ) ;
#14293 = DIRECTION ( 'NONE',  ( -0.000000000000000000, -0.000000000000000000, -1.000000000000000000 ) ) ;
#14295 = EDGE_CURVE ( 'NONE', #13487, #12691, #9396, .T. ) ;
#14294 = CARTESIAN_POINT ( 'NONE',  ( 44.55648932407425633, 156.6844580088725820, 38.96596240072933170 ) ) ;
#14296 = CARTESIAN_POINT ( 'NONE',  ( 40.27526882409969033, 143.9297705074273210, 30.44471234641811819 ) ) ;
#14297 = CARTESIAN_POINT ( 'NONE',  ( 32.75162935850930523, 152.6515011162663313, 2.501635869428501469 ) ) ;
#14298 = CIRCLE ( 'NONE', #20314, 5.000000000000004441 ) ;
#14299 = CARTESIAN_POINT ( 'NONE',  ( 40.27526882409969744, 128.6651871740940010, 30.44471234641812174 ) ) ;
#14300 = CIRCLE ( 'NONE', #7638, 10.00000000000000888 ) ;
#14301 = CARTESIAN_POINT ( 'NONE',  ( 138.2733499813809885, 177.2661675079481540, -44.99999999999997158 ) ) ;
#14302 = CARTESIAN_POINT ( 'NONE',  ( 173.3794444120442506, 0.000000000000000000, 30.00000000000000000 ) ) ;
#14303 = CYLINDRICAL_SURFACE ( 'NONE', #3401, 4.999999999999997335 ) ;
#14304 = VECTOR ( 'NONE', #11497, 1000.000000000000114 ) ;
#14305 = CARTESIAN_POINT ( 'NONE',  ( 44.55648932407425633, 149.8104996726487457, 29.45539723777780239 ) ) ;
#14306 = CARTESIAN_POINT ( 'NONE',  ( 32.01435502045076475, 93.85226834503447435, 6.866149820358673495 ) ) ;
#14307 = CARTESIAN_POINT ( 'NONE',  ( 38.01140435219952707, 120.7104996726487371, 34.21067981925357060 ) ) ;
#14308 = CARTESIAN_POINT ( 'NONE',  ( 47.43856463449117200, 109.7651871740939953, 32.77220824515698183 ) ) ;
#14309 = VERTEX_POINT ( 'NONE', #16013 ) ;
#14310 = LINE ( 'NONE', #8764, #14153 ) ;
#14311 = ORIENTED_EDGE ( 'NONE', *, *, #11249, .F. ) ;
#14312 = CARTESIAN_POINT ( 'NONE',  ( 43.01140435219951286, 95.03445800887259054, 28.95336869806222779 ) ) ;
#14313 = DIRECTION ( 'NONE',  ( 0.000000000000000000, 0.000000000000000000, -1.000000000000000000 ) ) ;
#14314 = VECTOR ( 'NONE', #8214, 1000.000000000000000 ) ;
#14315 = CARTESIAN_POINT ( 'NONE',  ( 48.01140435219951996, 152.2104996726487514, 34.21067981925357060 ) ) ;
#14317 = CARTESIAN_POINT ( 'NONE',  ( 69.09677972725788209, 109.4046064338026127, -6.910527774811301427 ) ) ;
#14316 = CARTESIAN_POINT ( 'NONE',  ( 40.27526882409969033, 105.5651871740939782, 37.97664729208901946 ) ) ;
#14318 = EDGE_CURVE ( 'NONE', #4323, #1933, #2573, .T. ) ;
#14319 = CARTESIAN_POINT ( 'NONE',  ( 41.46631938032478359, 61.31049967264873146, 38.96596240072933170 ) ) ;
#14321 = CARTESIAN_POINT ( 'NONE',  ( 43.80332655382220253, 61.95757658655229960, 29.21067981925356705 ) ) ;
#14320 = CARTESIAN_POINT ( 'NONE',  ( 47.50216252638477954, 144.5007669503875150, 31.98784611697848135 ) ) ;
#14322 =( NAMED_UNIT ( * ) PLANE_ANGLE_UNIT ( ) SI_UNIT ( $, .RADIAN. ) );
#14323 = DIRECTION ( 'NONE',  ( 0.000000000000000000, 1.000000000000000000, 0.000000000000000000 ) ) ;
#14324 = CARTESIAN_POINT ( 'NONE',  ( 44.55648932407425633, 146.8104996726487457, 29.45539723777780239 ) ) ;
#14325 = CARTESIAN_POINT ( 'NONE',  ( 44.37947211624943833, 70.01518717409399528, 38.42115945441014446 ) ) ;
#14326 = CARTESIAN_POINT ( 'NONE',  ( 53.88337135589062399, 152.3674195137575964, -9.803719146365084569 ) ) ;
#14327 = EDGE_CURVE ( 'NONE', #21028, #393, #7669, .T. ) ;
#14328 = CARTESIAN_POINT ( 'NONE',  ( -151.4692556286852607, -160.7391397928654442, 59.65701158161632378 ) ) ;
#14329 = CARTESIAN_POINT ( 'NONE',  ( -159.0959885057557983, -173.1938272943107506, 44.11586579668791330 ) ) ;
#14330 = LINE ( 'NONE', #2433, #18726 ) ;
#14331 = ORIENTED_EDGE ( 'NONE', *, *, #1239, .F. ) ;
#14332 = CARTESIAN_POINT ( 'NONE',  ( -154.3824083646099439, -181.5584106276440650, 58.62277379824867296 ) ) ;
#14333 = CIRCLE ( 'NONE', #12576, 10.00000000000000888 ) ;
#14334 = CARTESIAN_POINT ( 'NONE',  ( 76.86499250339331013, 125.5074929390188316, 4.406300711698651895 ) ) ;
#14335 = ORIENTED_EDGE ( 'NONE', *, *, #16732, .T. ) ;
#14336 = CARTESIAN_POINT ( 'NONE',  ( 41.64333658814960870, 129.7151871740940123, 38.42115945441014446 ) ) ;
#14337 = CARTESIAN_POINT ( 'NONE',  ( 44.37947211624943833, 155.2151871740940123, 30.00020018409699318 ) ) ;
#14338 = ORIENTED_EDGE ( 'NONE', *, *, #16206, .T. ) ;
#14339 = VERTEX_POINT ( 'NONE', #713 ) ;
#14340 = ADVANCED_FACE ( 'NONE', ( #18904 ), #2255, .F. ) ;
#14341 = CARTESIAN_POINT ( 'NONE',  ( 26.83015598135647295, 142.9878415585355071, 17.22988066553158149 ) ) ;
#14342 = VERTEX_POINT ( 'NONE', #4021 ) ;
#14343 = VECTOR ( 'NONE', #13399, 1000.000000000000000 ) ;
#14344 = CARTESIAN_POINT ( 'NONE',  ( 43.01140435219951996, 119.9070776186055838, -19.99999999999997868 ) ) ;
#14345 = CARTESIAN_POINT ( 'NONE',  ( 43.01140435219951286, 74.62977050742732388, 29.55568802177586463 ) ) ;
#14346 = CARTESIAN_POINT ( 'NONE',  ( 41.64333658814960870, 131.5151871740939953, 30.00020018409699318 ) ) ;
#14347 = VECTOR ( 'NONE', #2030, 1000.000000000000114 ) ;
#14348 = CARTESIAN_POINT ( 'NONE',  ( 46.10157429594899270, 94.76049967264873430, 38.46393386101376421 ) ) ;
#14349 = CARTESIAN_POINT ( 'NONE',  ( 72.98789752971651978, 103.3738663174133023, 6.148623012889737005 ) ) ;
#14350 = CARTESIAN_POINT ( 'NONE',  ( 42.21948215057684450, 60.03738109496900677, 29.21067981925356705 ) ) ;
#14351 = CARTESIAN_POINT ( 'NONE',  ( -157.6495955161842062, -158.9391397928654897, 41.15050349809590102 ) ) ;
#14352 = CARTESIAN_POINT ( 'NONE',  ( -151.4692556286852891, -196.9891397928655010, 49.65701158161630957 ) ) ;
#14353 = CARTESIAN_POINT ( 'NONE',  ( 48.01140435219951996, 64.13445800887257064, 35.83527830041809636 ) ) ;
#14354 = DIRECTION ( 'NONE',  ( 0.000000000000000000, 0.000000000000000000, 1.000000000000000000 ) ) ;
#14355 = ORIENTED_EDGE ( 'NONE', *, *, #12478, .T. ) ;
#14356 = CARTESIAN_POINT ( 'NONE',  ( 47.43856463449117200, 74.02977050742730114, 32.77220824515698183 ) ) ;
#14357 = CARTESIAN_POINT ( 'NONE',  ( -160.8964159109769696, -166.7438272943107336, 52.72008163687743121 ) ) ;
#14358 = CARTESIAN_POINT ( 'NONE',  ( 50.33192209904863290, 153.3481575868430014, -9.922832680162505525 ) ) ;
#14359 = CARTESIAN_POINT ( 'NONE',  ( -154.3824083646099439, -194.7584106276440536, 40.69124936498395328 ) ) ;
#14360 = ORIENTED_EDGE ( 'NONE', *, *, #601, .F. ) ;
#14361 = DIRECTION ( 'NONE',  ( -0.000000000000000000, 1.000000000000000000, -0.000000000000000000 ) ) ;
#14362 = CARTESIAN_POINT ( 'NONE',  ( 43.01140435219951286, 101.0344580088725621, 29.21067981925356705 ) ) ;
#14363 = CARTESIAN_POINT ( 'NONE',  ( 43.01140435219951286, 122.6297705074273239, 29.55568802177586107 ) ) ;
#14364 = ORIENTED_EDGE ( 'NONE', *, *, #17674, .T. ) ;
#14365 = AXIS2_PLACEMENT_3D ( 'NONE', #8434, #13279, #18345 ) ;
#14366 = ADVANCED_FACE ( 'NONE', ( #5989 ), #17453, .F. ) ;
#14367 = CARTESIAN_POINT ( 'NONE',  ( 38.29782421105369394, 159.5451350900380305, 34.21067981925357060 ) ) ;
#14368 = EDGE_LOOP ( 'NONE', ( #11294, #11402, #3918, #12115 ) ) ;
#14369 = CARTESIAN_POINT ( 'NONE',  ( 41.64333658814960870, 122.7797705074273296, 30.00020018409699318 ) ) ;
#14370 = MANIFOLD_SOLID_BREP ( 'Body-Move/Copy1', #2131 ) ;
#14371 = CARTESIAN_POINT ( 'NONE',  ( 48.01140435219951996, 134.0604996726486888, 35.83527830041809636 ) ) ;
#14372 = CARTESIAN_POINT ( 'NONE',  ( 41.46631938032478359, 99.11049967264872862, 29.45539723777780239 ) ) ;
#14373 = CARTESIAN_POINT ( 'NONE',  ( 93.25569916848381524, 126.0916958004080755, 4.000000000000003553 ) ) ;
#14374 = CARTESIAN_POINT ( 'NONE',  ( -159.5594255724347761, -176.1891397928654612, 55.53486410454104316 ) ) ;
#14375 = CARTESIAN_POINT ( 'NONE',  ( -151.4692556286852891, -190.7391397928654726, 60.17163382399899518 ) ) ;
#14376 = DIRECTION ( 'NONE',  ( -0.000000000000000000, -0.000000000000000000, -1.000000000000000000 ) ) ;
#14377 = FACE_OUTER_BOUND ( 'NONE', #3647, .T. ) ;
#14378 = CARTESIAN_POINT ( 'NONE',  ( -141.4692556286852891, -159.2130981290892748, 52.90620854394536821 ) ) ;
#14379 = SHAPE_DEFINITION_REPRESENTATION ( #16436, #14632 ) ;
#14380 = CARTESIAN_POINT ( 'NONE',  ( 38.01140435219951996, 134.9344580088725536, 35.83527830041810347 ) ) ;
#14381 = CARTESIAN_POINT ( 'NONE',  ( 39.42975644700377558, 102.6797705074273210, 36.81289934271958941 ) ) ;
#14382 = CARTESIAN_POINT ( 'NONE',  ( 62.56935518920172967, 140.3353681171158200, 3.771274953561639887 ) ) ;
#14383 = CARTESIAN_POINT ( 'NONE',  ( -159.0959885057557983, -193.5938272943107279, 55.19815736654470584 ) ) ;
#14384 = CARTESIAN_POINT ( 'NONE',  ( 38.58424406990786082, 93.11518717409400381, 34.21067981925357060 ) ) ;
#14385 = CARTESIAN_POINT ( 'NONE',  ( 41.46631938032478359, 90.11049967264874283, 29.45539723777780239 ) ) ;
#14386 = VERTEX_POINT ( 'NONE', #21657 ) ;
#14387 = CARTESIAN_POINT ( 'NONE',  ( 43.01140435219951996, 158.0344580088725763, 29.21067981925357060 ) ) ;
#14388 = CARTESIAN_POINT ( 'NONE',  ( 53.71239221804358976, 87.38980250447106357, 6.982120393166105998 ) ) ;
#14389 = CARTESIAN_POINT ( 'NONE',  ( 22.37680805599060818, 139.0098026693046336, -10.00581381704545514 ) ) ;
#14390 = EDGE_CURVE ( 'NONE', #14419, #2439, #4127, .T. ) ;
#14391 = CARTESIAN_POINT ( 'NONE',  ( 77.22348061889915982, 118.7203125366680752, -8.375138532479306619 ) ) ;
#14392 = CARTESIAN_POINT ( 'NONE',  ( 38.58424406990785371, 75.52977050742732956, 35.64915139335015937 ) ) ;
#14393 = ORIENTED_EDGE ( 'NONE', *, *, #14198, .T. ) ;
#14394 = ORIENTED_EDGE ( 'NONE', *, *, #9609, .F. ) ;
#14395 = CARTESIAN_POINT ( 'NONE',  ( 46.59305225739526435, 154.5797705074273267, 36.81289934271958941 ) ) ;
#14396 = AXIS2_PLACEMENT_3D ( 'NONE', #6829, #7477, #4051 ) ;
#14397 = CARTESIAN_POINT ( 'NONE',  ( 145.5008360144876747, 198.5836349573982886, 34.00000000000001421 ) ) ;
#14398 = CARTESIAN_POINT ( 'NONE',  ( 39.92123440845004723, 121.1604996726487400, 38.46393386101376421 ) ) ;
#14400 = CARTESIAN_POINT ( 'NONE',  ( 20.11427441861009058, 94.56644311770523359, -4.846896973145477183 ) ) ;
#14399 = CARTESIAN_POINT ( 'NONE',  ( 39.42975644700377558, 78.41518717409400097, 36.81289934271958941 ) ) ;
#14401 = EDGE_CURVE ( 'NONE', #10776, #4102, #7987, .T. ) ;
#14402 = CARTESIAN_POINT ( 'NONE',  ( -160.8964159109769696, -175.7438272943107052, 52.72008163687743121 ) ) ;
#14403 = CARTESIAN_POINT ( 'NONE',  ( 46.10157429594899270, 112.7604996726487485, 38.46393386101375711 ) ) ;
#14404 = CARTESIAN_POINT ( 'NONE',  ( -141.4692556286852891, -191.9130981290893203, 46.40781461928724383 ) ) ;
#14405 = CARTESIAN_POINT ( 'NONE',  ( 18.67254549292281496, -61.68114226949890622, -16.21320343559643717 ) ) ;
#14406 = LINE ( 'NONE', #16166, #4801 ) ;
#14407 = CARTESIAN_POINT ( 'NONE',  ( 46.59305225739526435, 145.5797705074273267, 36.81289934271958941 ) ) ;
#14408 =( BOUNDED_CURVE ( )  B_SPLINE_CURVE ( 2, ( #8551, #16686, #3253, #1818, #5233, #13499, #6792, #18783, #20553, #20230, #15479, #5124, #10414 ),
 .UNSPECIFIED., .F., .F. ) 
 B_SPLINE_CURVE_WITH_KNOTS ( ( 3, 2, 2, 2, 2, 2, 3 ),
 ( 0.8014705882352941568, 0.8029411764705882693, 0.8058823529411764941, 0.8088235294117647189, 0.8117647058823529438, 0.8147058823529411686, 0.8161764705882352811 ),
 .UNSPECIFIED. ) 
 CURVE ( )  GEOMETRIC_REPRESENTATION_ITEM ( )  RATIONAL_B_SPLINE_CURVE ( ( 0.9755282581475768211, 0.9755282581475768211, 1.000000000000000000, 0.9510565162951535312, 1.000000000000000000, 0.9510565162951535312, 1.000000000000000000, 0.9510565162951535312, 1.000000000000000000, 0.9510565162951535312, 1.000000000000000000, 0.9755282581475768211, 0.9755282581475768211 ) ) 
 REPRESENTATION_ITEM ( '' )  );
#14409 = CARTESIAN_POINT ( 'NONE',  ( 51.83766784316492249, 86.74794057323931895, -0.9509610611041249273 ) ) ;
#14410 = CARTESIAN_POINT ( 'NONE',  ( 41.64333658814960870, 125.5151871740939953, 30.00020018409699318 ) ) ;
#14411 =( NAMED_UNIT ( * ) PLANE_ANGLE_UNIT ( ) SI_UNIT ( $, .RADIAN. ) );
#14412 = CARTESIAN_POINT ( 'NONE',  ( 42.21948215057683740, 151.3836182503284817, 39.21067981925355639 ) ) ;
#14413 = MECHANICAL_DESIGN_GEOMETRIC_PRESENTATION_REPRESENTATION (  '', ( #10561 ), #5615 ) ;
#14414 = CARTESIAN_POINT ( 'NONE',  ( 149.5529451524149920, 187.4828467975320336, 34.00000000000001421 ) ) ;
#14415 = DIRECTION ( 'NONE',  ( 1.000000000000000000, 0.000000000000000000, 0.000000000000000000 ) ) ;
#14416 = CARTESIAN_POINT ( 'NONE',  ( 33.70380864093198170, 93.20109254516876263, 20.79496611990781929 ) ) ;
#14417 = DIRECTION ( 'NONE',  ( 0.000000000000000000, 0.000000000000000000, 1.000000000000000000 ) ) ;
#14418 = CARTESIAN_POINT ( 'NONE',  ( 40.27526882409969033, 108.5651871740939924, 37.97664729208901946 ) ) ;
#14419 = VERTEX_POINT ( 'NONE', #1250 ) ;
#14420 = CARTESIAN_POINT ( 'NONE',  ( -143.3790856849358306, -156.6891397928654612, 43.77915905869157598 ) ) ;
#14421 = ORIENTED_EDGE ( 'NONE', *, *, #4976, .T. ) ;
#14422 = CARTESIAN_POINT ( 'NONE',  ( 48.01140435219951996, 94.28445800887259054, 34.21067981925357060 ) ) ;
#14423 = CARTESIAN_POINT ( 'NONE',  ( -151.4692556286852891, -126.9891397928655010, -54.65701158161630246 ) ) ;
#14424 = AXIS2_PLACEMENT_3D ( 'NONE', #3610, #13946, #8789 ) ;
#14425 = CARTESIAN_POINT ( 'NONE',  ( 47.05648932407426344, 151.9104996726487400, 37.14960608071593384 ) ) ;
#14427 = CARTESIAN_POINT ( 'NONE',  ( 26.87902611899987448, 142.9395564687116007, -9.767670631928341507 ) ) ;
#14426 = CARTESIAN_POINT ( 'NONE',  ( 39.42975644700377558, 105.4151871740940152, 36.81289934271958941 ) ) ;
#14428 = CARTESIAN_POINT ( 'NONE',  ( 38.01140435219951996, 63.56049967264873146, 32.58608133808903773 ) ) ;
#14430 = CYLINDRICAL_SURFACE ( 'NONE', #10088, 4.999999999999997335 ) ;
#14429 = CARTESIAN_POINT ( 'NONE',  ( 31.20897972572456069, 148.4098837309091721, 17.43780275515692679 ) ) ;
#14431 = DIRECTION ( 'NONE',  ( 0.000000000000000000, 1.000000000000000000, 0.000000000000000000 ) ) ;
#14432 = CYLINDRICAL_SURFACE ( 'NONE', #10726, 4.999999999999997335 ) ;
#14433 = CARTESIAN_POINT ( 'NONE',  ( 2.004595370269653287, 635.3380690778678854, -0.8325491102011938205 ) ) ;
#14434 = CARTESIAN_POINT ( 'NONE',  ( 39.42975644700377558, 72.41518717409400097, 36.81289934271958941 ) ) ;
#14435 = CARTESIAN_POINT ( 'NONE',  ( 36.55618291757107841, 153.5264344809625641, -3.375052104409746789 ) ) ;
#14436 = CARTESIAN_POINT ( 'NONE',  ( 48.01140435219951996, 95.36049967264872862, 32.58608133808903773 ) ) ;
#14437 = CARTESIAN_POINT ( 'NONE',  ( -160.8964159109769696, -166.8938272943107393, 49.65701158161630957 ) ) ;
#14438 = CARTESIAN_POINT ( 'NONE',  ( -151.4692556286852891, -185.9084106276440025, 39.74470866294723947 ) ) ;
#14439 = VERTEX_POINT ( 'NONE', #6432 ) ;
#14440 = CARTESIAN_POINT ( 'NONE',  ( -157.2955611005346270, -169.7084106276440139, 57.67623309621198047 ) ) ;
#14441 = CARTESIAN_POINT ( 'NONE',  ( 77.32109437525961937, 120.4276527761501399, 18.57288864564252506 ) ) ;
#14442 = VERTEX_POINT ( 'NONE', #4774 ) ;
#14443 = CARTESIAN_POINT ( 'NONE',  ( 47.43856463449117200, 136.7651871740939953, 32.77220824515698183 ) ) ;
#14444 = EDGE_CURVE ( 'NONE', #8092, #13745, #5149, .T. ) ;
#14445 = CARTESIAN_POINT ( 'NONE',  ( 44.37947211624943833, 92.47977050742731819, 30.00020018409699318 ) ) ;
#14446 = ORIENTED_EDGE ( 'NONE', *, *, #9404, .T. ) ;
#14447 = ORIENTED_EDGE ( 'NONE', *, *, #21316, .F. ) ;
#14448 = CARTESIAN_POINT ( 'NONE',  ( 29.48178659935447854, 144.5857871963822845, 17.33364154221121467 ) ) ;
#14449 = ORIENTED_EDGE ( 'NONE', *, *, #10032, .F. ) ;
#14450 = FACE_BOUND ( 'NONE', #21019, .T. ) ;
#14451 = CARTESIAN_POINT ( 'NONE',  ( 47.43856463449118621, 73.87977050742732388, 34.21067981925357060 ) ) ;
#14452 = CARTESIAN_POINT ( 'NONE',  ( 38.58424406990786082, 132.1151871740940180, 34.21067981925357060 ) ) ;
#14453 = CARTESIAN_POINT ( 'NONE',  ( 44.55648932407425633, 88.61049967264874283, 38.96596240072933170 ) ) ;
#14454 = CARTESIAN_POINT ( 'NONE',  ( 9.822352152143091431, 128.2981216602131553, 9.363167623699879982 ) ) ;
#14455 = CYLINDRICAL_SURFACE ( 'NONE', #5092, 4.999999999999997335 ) ;
#14456 = CARTESIAN_POINT ( 'NONE',  ( -154.5594255724347761, -157.8891397928654783, 59.16757674456785310 ) ) ;
#14457 = CARTESIAN_POINT ( 'NONE',  ( 48.01140435219951996, 107.0604996726487457, 35.83527830041809636 ) ) ;
#14458 = CARTESIAN_POINT ( 'NONE',  ( 46.10157429594899270, 61.76049967264874141, 38.46393386101375711 ) ) ;
#14459 = ORIENTED_EDGE ( 'NONE', *, *, #1943, .F. ) ;
#14460 = CARTESIAN_POINT ( 'NONE',  ( 45.74753988029933538, 74.32977050742729830, 30.44471234641811819 ) ) ;
#14461 = CARTESIAN_POINT ( 'NONE',  ( -151.4692556286852891, -158.6438272943107108, 39.74470866294723947 ) ) ;
#14462 = CARTESIAN_POINT ( 'NONE',  ( 10.42839491720816625, 130.4056617841633283, -4.565575592310756825 ) ) ;
#14463 = FACE_OUTER_BOUND ( 'NONE', #11516, .T. ) ;
#14464 = ORIENTED_EDGE ( 'NONE', *, *, #1391, .F. ) ;
#14465 = LINE ( 'NONE', #13150, #1979 ) ;
#14466 = CARTESIAN_POINT ( 'NONE',  ( 44.55648932407425633, 123.6844580088725820, 38.96596240072933170 ) ) ;
#14467 =( BOUNDED_CURVE ( )  B_SPLINE_CURVE ( 2, ( #5929, #12659, #21151, #19380, #4275 ),
 .UNSPECIFIED., .F., .F. ) 
 B_SPLINE_CURVE_WITH_KNOTS ( ( 3, 2, 3 ),
 ( 0.9464285714285713969, 0.9499999999999999556, 0.9523897249335829818 ),
 .UNSPECIFIED. ) 
 CURVE ( )  GEOMETRIC_REPRESENTATION_ITEM ( )  RATIONAL_B_SPLINE_CURVE ( ( 0.9755282581475768211, 0.9755282581475768211, 1.000000000000000000, 0.9836253951315760968, 0.9782074146920120006 ) ) 
 REPRESENTATION_ITEM ( '' )  );
#14468 = ADVANCED_FACE ( 'NONE', ( #1144 ), #4553, .T. ) ;
#14469 = CARTESIAN_POINT ( 'NONE',  ( 45.74753988029934249, 127.4297705074273352, 37.97664729208901235 ) ) ;
#14470 = ORIENTED_EDGE ( 'NONE', *, *, #9771, .T. ) ;
#14471 = ORIENTED_EDGE ( 'NONE', *, *, #1773, .T. ) ;
#14472 = CARTESIAN_POINT ( 'NONE',  ( 39.42975644700377558, 129.0797705074273267, 31.60846029578754468 ) ) ;
#14473 = CARTESIAN_POINT ( 'NONE',  ( 43.01140435219951286, 73.46049967264872294, 39.21067981925356349 ) ) ;
#14474 = CARTESIAN_POINT ( 'NONE',  ( 38.96631938032478359, 59.48445800887257207, 31.27175355779120025 ) ) ;
#14475 = VECTOR ( 'NONE', #1408, 1000.000000000000000 ) ;
#14476 = VECTOR ( 'NONE', #2015, 1000.000000000000000 ) ;
#14477 = CARTESIAN_POINT ( 'NONE',  ( -156.4692864601533131, -155.0638355923473455, 40.99677534440144200 ) ) ;
#14478 = DIRECTION ( 'NONE',  ( 1.000000000000000000, 0.000000000000000000, 0.000000000000000000 ) ) ;
#14479 = LINE ( 'NONE', #2580, #2800 ) ;
#14480 = CARTESIAN_POINT ( 'NONE',  ( -159.5594255724347761, -185.7891397928654840, 43.77915905869157598 ) ) ;
#14481 = CARTESIAN_POINT ( 'NONE',  ( 43.80332655382220253, 133.9575765865523067, 29.21067981925356705 ) ) ;
#14482 = CARTESIAN_POINT ( 'NONE',  ( 43.01140435219951286, 130.4604996726487229, 39.21067981925356349 ) ) ;
#14483 = CARTESIAN_POINT ( 'NONE',  ( -160.8964159109769696, -190.7438272943107336, 52.72008163687743121 ) ) ;
#14484 = PRODUCT_CONTEXT ( 'NONE', #4779, 'mechanical' ) ;
#14485 = AXIS2_PLACEMENT_3D ( 'NONE', #410, #5151, #17149 ) ;
#14486 = EDGE_CURVE ( 'NONE', #14386, #18391, #11859, .T. ) ;
#14487 = EDGE_CURVE ( 'NONE', #9553, #9751, #14578, .T. ) ;
#14488 = CARTESIAN_POINT ( 'NONE',  ( 47.05648932407426344, 136.5844580088725877, 31.27175355779120025 ) ) ;
#14489 = CARTESIAN_POINT ( 'NONE',  ( 46.59305225739526435, 101.1797705074273210, 31.60846029578754468 ) ) ;
#14490 = CARTESIAN_POINT ( 'NONE',  ( 49.77943037783704483, 92.44786530929899016, 6.152137702922222395 ) ) ;
#14491 = CARTESIAN_POINT ( 'NONE',  ( -157.2955611005346270, -194.3438272943106995, 41.63779006702063867 ) ) ;
#14492 = CARTESIAN_POINT ( 'NONE',  ( 47.43856463449117911, 100.4651871740939981, 35.64915139335015937 ) ) ;
#14493 = CARTESIAN_POINT ( 'NONE',  ( 141.1725454929228079, -61.68114226949890622, -46.21320343559645494 ) ) ;
#14494 = ORIENTED_EDGE ( 'NONE', *, *, #16312, .F. ) ;
#14495 = CARTESIAN_POINT ( 'NONE',  ( 47.05648932407426344, 127.9104996726487542, 37.14960608071593384 ) ) ;
#14496 = CARTESIAN_POINT ( 'NONE',  ( 64.11693453485118255, 146.8606268255622638, -2.422805558527139080 ) ) ;
#14497 = CARTESIAN_POINT ( 'NONE',  ( 52.67254683800726411, 146.3150465326280028, -8.696212858991016148 ) ) ;
#14498 = CARTESIAN_POINT ( 'NONE',  ( 60.49690154327523572, 149.3382625450468311, -9.565656633516235630 ) ) ;
#14499 = MECHANICAL_DESIGN_GEOMETRIC_PRESENTATION_REPRESENTATION (  '', ( #10302 ), #4656 ) ;
#14500 = CARTESIAN_POINT ( 'NONE',  ( 39.42975644700377558, 63.67977050742732104, 36.81289934271958941 ) ) ;
#14501 = ORIENTED_EDGE ( 'NONE', *, *, #3566, .F. ) ;
#14502 = ORIENTED_EDGE ( 'NONE', *, *, #15611, .T. ) ;
#14503 = LINE ( 'NONE', #9239, #16790 ) ;
#14504 = CIRCLE ( 'NONE', #17320, 7.500000000000007105 ) ;
#14505 = CARTESIAN_POINT ( 'NONE',  ( -153.0531000319306827, -194.2362167067690564, 39.65701158161629536 ) ) ;
#14506 = CARTESIAN_POINT ( 'NONE',  ( 38.01140435219952707, 123.7104996726487371, 34.21067981925357060 ) ) ;
#14508 = CARTESIAN_POINT ( 'NONE',  ( 12.60192345832597027, 135.3850619972812979, 10.60811072801600119 ) ) ;
#14507 = CARTESIAN_POINT ( 'NONE',  ( 46.59305225739526435, 82.31518717409400665, 36.81289934271958941 ) ) ;
#14509 = CARTESIAN_POINT ( 'NONE',  ( 43.01140435219951286, 95.03445800887257633, 29.21067981925356705 ) ) ;
#14510 = CARTESIAN_POINT ( 'NONE',  ( -154.3824083646099439, -173.4938272943107336, 40.69124936498395328 ) ) ;
#14511 = CARTESIAN_POINT ( 'NONE',  ( 55.94180145820917716, 151.6039095241057453, 11.26783467880839140 ) ) ;
#14512 = CARTESIAN_POINT ( 'NONE',  ( -154.5594255724347761, -188.1630981290893203, 40.14644641866476604 ) ) ;
#14513 = EDGE_CURVE ( 'NONE', #872, #15251, #10456, .T. ) ;
#14514 = FACE_BOUND ( 'NONE', #15024, .T. ) ;
#14515 = CARTESIAN_POINT ( 'NONE',  ( -94.10404323627655288, -13.18023274290474767, 4.000000000000021316 ) ) ;
#14516 = CARTESIAN_POINT ( 'NONE',  ( 46.59305225739526435, 137.1797705074273210, 31.60846029578754468 ) ) ;
#14517 = CARTESIAN_POINT ( 'NONE',  ( 10.28555834757860055, 130.2242880576791890, 1.430031502841225821 ) ) ;
#14518 = CARTESIAN_POINT ( 'NONE',  ( 44.37947211624943833, 130.0151871740939953, 38.42115945441014446 ) ) ;
#14519 = PRESENTATION_STYLE_ASSIGNMENT (( #5926 ) ) ;
#14520 = CARTESIAN_POINT ( 'NONE',  ( 38.96631938032478359, 150.4104996726487400, 31.27175355779120025 ) ) ;
#14521 = DIRECTION ( 'NONE',  ( 0.000000000000000000, 0.000000000000000000, 1.000000000000000000 ) ) ;
#14522 = CARTESIAN_POINT ( 'NONE',  ( 147.5268905834513475, 193.0332408774651185, -49.99999999999997158 ) ) ;
#14523 = CARTESIAN_POINT ( 'NONE',  ( 26.70363248220801466, 142.8423586596025245, -10.77201286955609127 ) ) ;
#14524 = CARTESIAN_POINT ( 'NONE',  ( 41.46631938032478359, 120.1104996726487570, 29.45539723777780239 ) ) ;
#14525 = CARTESIAN_POINT ( 'NONE',  ( 45.74753988029933538, 109.1651871740939868, 37.97664729208901946 ) ) ;
#14526 = EDGE_LOOP ( 'NONE', ( #2049, #5425, #3997, #5501 ) ) ;
#14527 = DIRECTION ( 'NONE',  ( -0.000000000000000000, 1.000000000000000000, -0.000000000000000000 ) ) ;
#14528 = ORIENTED_EDGE ( 'NONE', *, *, #19865, .T. ) ;
#14529 = CARTESIAN_POINT ( 'NONE',  ( 48.01140435219951996, 85.28445800887257633, 34.21067981925357060 ) ) ;
#14530 = DIRECTION ( 'NONE',  ( -0.000000000000000000, -0.000000000000000000, -1.000000000000000000 ) ) ;
#14531 = CARTESIAN_POINT ( 'NONE',  ( 38.01140435219951996, 147.5604996726487457, 32.58608133808903773 ) ) ;
#14533 = CARTESIAN_POINT ( 'NONE',  ( 37.37095630934955892, 92.35886976769425871, -5.362784416626555029 ) ) ;
#14532 = CARTESIAN_POINT ( 'NONE',  ( 45.74753988029933538, 104.0651871740940067, 30.44471234641811819 ) ) ;
#14534 = CARTESIAN_POINT ( 'NONE',  ( 44.55648932407425633, 65.81049967264873146, 29.45539723777780239 ) ) ;
#14536 = CARTESIAN_POINT ( 'NONE',  ( 173.3794444120442506, -126.9891397928655010, -17.64809332337413750 ) ) ;
#14535 = CARTESIAN_POINT ( 'NONE',  ( 47.34826785674352578, 144.5287207813994996, 31.70117790783977796 ) ) ;
#14537 = CARTESIAN_POINT ( 'NONE',  ( 48.01140435219951996, 118.1344580088725849, 35.83527830041809636 ) ) ;
#14538 = CARTESIAN_POINT ( 'NONE',  ( 47.05648932407426344, 79.58445800887257349, 31.27175355779120025 ) ) ;
#14539 = CARTESIAN_POINT ( 'NONE',  ( -151.4692556286852891, -189.8130981290892976, 59.65701158161632378 ) ) ;
#14540 = CARTESIAN_POINT ( 'NONE',  ( 43.01140435219951286, 62.36518717409399670, 29.55568802177586463 ) ) ;
#14541 = FACE_OUTER_BOUND ( 'NONE', #13988, .T. ) ;
#14542 = CARTESIAN_POINT ( 'NONE',  ( 44.37947211624943833, 152.2151871740940123, 30.00020018409699318 ) ) ;
#14543 = FACE_OUTER_BOUND ( 'NONE', #10823, .T. ) ;
#14544 = CARTESIAN_POINT ( 'NONE',  ( -142.0420953463935803, -171.2438272943107052, 46.59394152635518793 ) ) ;
#14545 = CARTESIAN_POINT ( 'NONE',  ( -142.0420953463935803, -180.8084106276440366, 52.72008163687743831 ) ) ;
#14546 = ORIENTED_EDGE ( 'NONE', *, *, #16615, .F. ) ;
#14547 = CARTESIAN_POINT ( 'NONE',  ( 41.64333658814960870, 65.51518717409400949, 30.00020018409699318 ) ) ;
#14548 = CARTESIAN_POINT ( 'NONE',  ( -160.8964159109769696, -167.1584106276440593, 49.65701158161630957 ) ) ;
#14549 = MANIFOLD_SOLID_BREP ( 'Sweep1', #17939 ) ;
#14550 = CARTESIAN_POINT ( 'NONE',  ( 72.28893465744093305, 137.8051215927966382, 17.97743314940082371 ) ) ;
#14551 = DIRECTION ( 'NONE',  ( 0.5000000000000004441, 0.000000000000000000, 0.8660254037844383745 ) ) ;
#14552 = CARTESIAN_POINT ( 'NONE',  ( 45.74753988029933538, 139.1651871740940010, 37.97664729208901946 ) ) ;
#14553 = EDGE_LOOP ( 'NONE', ( #19386, #7762, #1363, #19537 ) ) ;
#14554 = ORIENTED_EDGE ( 'NONE', *, *, #7877, .T. ) ;
#14555 = CARTESIAN_POINT ( 'NONE',  ( 17.81206540393426252, 132.5069038242342003, 16.68302557436956945 ) ) ;
#14556 = ORIENTED_EDGE ( 'NONE', *, *, #3947, .F. ) ;
#14557 = DIRECTION ( 'NONE',  ( 0.000000000000000000, 0.000000000000000000, 1.000000000000000000 ) ) ;
#14558 = CARTESIAN_POINT ( 'NONE',  ( 44.37947211624943833, 80.47977050742731819, 30.00020018409699318 ) ) ;
#14559 = CARTESIAN_POINT ( 'NONE',  ( 45.74753988029933538, 140.0651871740940067, 30.44471234641811819 ) ) ;
#14560 = CARTESIAN_POINT ( 'NONE',  ( 38.96631938032478359, 87.41049967264873999, 31.27175355779120025 ) ) ;
#14561 = CARTESIAN_POINT ( 'NONE',  ( 32.14050509837299785, 87.44534670509604268, 7.696117750009315195 ) ) ;
#14562 = CARTESIAN_POINT ( 'NONE',  ( 38.17059775574655589, 95.38013743195961069, 35.50423386912937218 ) ) ;
#14563 = CARTESIAN_POINT ( 'NONE',  ( -143.3790856849358306, -157.2891397928654555, 55.53486410454105027 ) ) ;
#14564 = CARTESIAN_POINT ( 'NONE',  ( 144.5586921005913439, 160.7104996726487798, -19.99999999999999645 ) ) ;
#14565 = FACE_OUTER_BOUND ( 'NONE', #13846, .T. ) ;
#14566 = EDGE_CURVE ( 'NONE', #10804, #18715, #7260, .T. ) ;
#14567 = ORIENTED_EDGE ( 'NONE', *, *, #14513, .F. ) ;
#14568 = CARTESIAN_POINT ( 'NONE',  ( 44.37947211624943833, 71.47977050742731819, 30.00020018409699318 ) ) ;
#14569 = CARTESIAN_POINT ( 'NONE',  ( -145.6429501568359797, -193.1084106276440480, 57.67623309621198047 ) ) ;
#14570 = CARTESIAN_POINT ( 'NONE',  ( 18.20936163119166196, 143.5026679720446907, 2.934308097026923967 ) ) ;
#14571 = CARTESIAN_POINT ( 'NONE',  ( -145.6429501568359797, -187.1084106276440480, 57.67623309621198047 ) ) ;
#14572 = VERTEX_POINT ( 'NONE', #12801 ) ;
#14573 = CARTESIAN_POINT ( 'NONE',  ( -159.5594255724347761, -161.7891397928654555, 43.77915905869157598 ) ) ;
#14574 = CARTESIAN_POINT ( 'NONE',  ( 48.01140435219951996, 124.2844580088725905, 34.21067981925357060 ) ) ;
#14575 = CIRCLE ( 'NONE', #850, 15.56217413224114310 ) ;
#14576 = CARTESIAN_POINT ( 'NONE',  ( 47.43856463449117911, 122.0297705074273154, 32.77220824515697473 ) ) ;
#14577 = ORIENTED_EDGE ( 'NONE', *, *, #6191, .T. ) ;
#14578 = LINE ( 'NONE', #2794, #20660 ) ;
#14579 = ORIENTED_EDGE ( 'NONE', *, *, #17944, .T. ) ;
#14580 = CARTESIAN_POINT ( 'NONE',  ( 47.43856463449118621, 127.8797705074273239, 34.21067981925357060 ) ) ;
#14581 = MANIFOLD_SOLID_BREP ( 'Cut-Extrude9', #20437 ) ;
#14582 = FACE_OUTER_BOUND ( 'NONE', #17322, .T. ) ;
#14583 = CARTESIAN_POINT ( 'NONE',  ( 39.92123440845004723, 68.33445800887258770, 29.95742577749337343 ) ) ;
#14584 = EDGE_CURVE ( 'NONE', #12691, #4603, #18744, .T. ) ;
#14585 = CARTESIAN_POINT ( 'NONE',  ( 43.01140435219951996, 10.71049967264875491, 34.21067981925357060 ) ) ;
#14586 = CARTESIAN_POINT ( 'NONE',  ( 42.21948215057684450, 101.1113394311928460, 29.21067981925356705 ) ) ;
#14587 = CARTESIAN_POINT ( 'NONE',  ( -154.5594255724347761, -175.8891397928654783, 59.16757674456785310 ) ) ;
#14588 = CARTESIAN_POINT ( 'NONE',  ( -157.6495955161842062, -188.9391397928654612, 41.15050349809590102 ) ) ;
#14589 = EDGE_CURVE ( 'NONE', #2680, #21236, #17313, .T. ) ;
#14590 = DIRECTION ( 'NONE',  ( -0.000000000000000000, -0.000000000000000000, -1.000000000000000000 ) ) ;
#14591 = CARTESIAN_POINT ( 'NONE',  ( 43.80332655382220253, 130.5373810949689926, 39.21067981925355639 ) ) ;
#14592 = CARTESIAN_POINT ( 'NONE',  ( -145.6429501568359797, -191.9438272943106938, 41.63779006702063867 ) ) ;
#14593 = CARTESIAN_POINT ( 'NONE',  ( 46.10157429594899270, 124.7344580088725792, 29.95742577749337343 ) ) ;
#14594 = CARTESIAN_POINT ( 'NONE',  ( 47.43856463449117200, 100.7297705074273040, 35.64915139335016647 ) ) ;
#14595 =( BOUNDED_SURFACE ( )  B_SPLINE_SURFACE ( 3, 3, ( 
 ( #7661, #12383, #2567, #4013, #12603, #4225, #10636, #14358, #17443, #2354, #7765, #19220, #9092, #2670, #809, #8981, #17340, #17550, #19325, #5765, #703, #4326, #12816, #19118, #12709, #2459, #10953, #7334, #16004, #6088, #7546, #915, #19535, #9414, #9199, #15897, #16122, #14462, #19432, #7437, #14244, #21099, #4118, #20988, #11051, #17766, #17661, #15794, #1028, #9304, #21205, #5873, #5982, #2247, #20769, #14034, #5660, #14140, #20877, #12493, #10854, #16334, #14684, #3228, #21424, #12929, #9528, #9849, #1355, #13259, #16665, #18213, #13147, #6538, #17874, #11161, #19996, #11376, #6313, #14570, #18097, #1243, #4880, #14899, #1466, #3007, #16225, #21752, #9744, #16550, #1136, #9962, #8198, #7977, #21647, #11599, #7871, #21312, #3118, #6197, #6662, #19653, #1576, #18329, #4544, #8304, #11266, #6425, #19876, #4429, #15012, #17985, #2899, #13369, #13040, #9634, #2785, #16441, #19764, #4661, #8086, #4763, #14793, #21535, #11484, #462, #6768, #359, #5213, #20420, #10068, #3665, #15558, #10284, #10395, #7194, #12134, #18656, #11927, #18867, #17200, #7087, #10180, #1896, #8742, #13578, #3560, #20530, #5416, #5317, #3457, #3775, #12030, #13790, #8632, #13686, #2115, #8417, #6983, #20106, #17095, #18764 ),
 ( #11819, #11705, #16881, #3340, #2010, #30, #8852, #15459, #4995, #10503, #18441, #20209, #16989, #16777, #1687, #15127, #13477, #20315, #5103, #15350, #18551, #1798, #140, #8529, #15242, #6870, #245, #4093, #15981, #7414, #5519, #20742, #5847, #3991, #4302, #18979, #14222, #9064, #17635, #8954, #10826, #9388, #17741, #2646, #5630, #9280, #2543, #891, #4200, #16093, #17311, #7630, #1003, #3882, #14334, #12577, #14008, #5741, #11028, #2325, #21074, #2223, #15660, #785, #12355, #15772, #19091, #2435, #563, #5956, #17525, #9174, #15873, #10716, #12249, #13898, #20962, #10607, #676, #10928, #19302, #7308, #7521, #12682, #20637, #17419, #14113, #19405, #20851, #12465, #19196, #16524, #9717, #9936, #21621, #12904, #9503, #13125, #17852, #21292, #21175, #19626, #12793, #19847, #16200, #18303, #8061, #4854, #19970, #4738, #7847, #4630, #3205, #6066, #6512, #16641, #1220, #4405, #19737, #1442, #9826, #9611, #8171, #1112, #11574, #7740, #11349, #14876, #7953, #19513, #14550, #21512, #4520, #14441, #11137, #14769, #2867, #16418, #18072, #1328, #2763, #6170, #6397, #3093, #13232, #11242, #11457, #17962, #16309, #14658, #21398, #6286, #13017, #2979, #18186, #18739, #5395, #8282, #20507, #15217, #4970, #18419 ),
 ( #1551, #13454, #11794, #332, #18524, #10046, #6633, #6955, #20290, #10369, #13766, #15326, #10261, #3642, #14983, #21728, #17069, #3433, #8504, #12112, #20083, #6746, #18843, #3750, #10479, #5080, #10155, #13662, #20188, #16856, #20396, #8716, #1770, #13346, #15434, #1983, #116, #16963, #7061, #11903, #16750, #219, #6847, #13555, #11682, #5184, #18632, #3317, #12005, #5291, #3536, #1659, #8392, #1875, #15101, #5, #8606, #20938, #7282, #12551, #14199, #440, #5495, #15849, #20612, #19381, #7170, #14306, #5818, #18956, #9151, #10583, #19169, #10798, #17179, #19277, #17285, #2200, #21048, #3967, #8930, #9256, #7391, #15534, #2093, #2298, #4069, #12329, #13981, #10907, #4276, #3858, #4178, #9040, #17501, #13874, #760, #12660, #14090, #7497, #8825, #15956, #15750, #654, #869, #5930, #17610, #20719, #20826, #2516, #10690, #5718, #7603, #12223, #2412, #540, #15636, #5604, #19065, #12442, #17396, #8141, #21152, #19710, #11005, #8035, #17930, #1086, #13095, #21481, #14743, #9581, #974, #6481, #2840, #16388, #7715, #9802, #6369, #7818, #19821, #4711, #16064, #6037, #9691, #14416, #13201, #12766, #14845, #11429, #19487, #2950, #4379, #12988, #4601, #17715, #18155, #11110, #17826, #21590, #19596, #2735 ),
 ( #11320, #6142, #14523, #3062, #19937, #9475, #16494, #16285, #18044, #16175, #1301, #2620, #1191, #1413, #9360, #21263, #7924, #14628, #12875, #4489, #11214, #21367, #6256, #15297, #20161, #11763, #5266, #11982, #5156, #10015, #18712, #11875, #6928, #8479, #20264, #1956, #14954, #13529, #4823, #1850, #18606, #16831, #11546, #16719, #15073, #3619, #21809, #13318, #9905, #10234, #1743, #13633, #17044, #3510, #16935, #20370, #18273, #3176, #10341, #6718, #18494, #8686, #1523, #1629, #15410, #307, #13741, #8362, #13424, #8581, #5051, #3399, #190, #7035, #10125, #16610, #8252, #21700, #15186, #6600, #20054, #89, #4941, #11651, #6821, #18386, #3286, #9233, #7578, #2170, #519, #4045, #17259, #13956, #10772, #5795, #20694, #17585, #12526, #7467, #8908, #7364, #14175, #9013, #7146, #19145, #5577, #15610, #8799, #12301, #10558, #739, #9125, #17480, #19041, #10452, #15932, #3937, #2389, #17153, #19252, #15824, #7255, #20909, #4154, #3723, #15512, #10884, #2070, #843, #414, #2492, #20479, #13850, #12416, #20585, #628, #14066, #5371, #12087, #5471, #12195, #18817, #10667, #18931, #3831, #17370, #2274, #15725, #20801, #5692, #9451, #4354, #8012, #16472, #948, #16366, #21240, #14604, #4254, #19685, #9777 ),
 ( #17906, #11194, #2818, #12742, #12635, #1388, #21343, #10980, #2707, #11297, #12962, #19356, #7901, #1277, #14278, #17693, #11083, #18020, #2930, #9666, #6231, #14719, #16259, #21023, #6344, #19464, #16034, #4576, #2595, #6012, #5905, #17797, #9334, #21454, #7693, #3038, #13070, #11405, #4688, #19798, #14389, #9556, #21129, #16151, #18129, #1060, #7793, #14497, #6118, #12848, #19568, #4462, #1168, #1829, #10214, #9994, #8561, #16580, #20349, #8117, #20135, #16916, #1605, #21566, #14932, #61, #20032, #5244, #13179, #8456, #3262, #10100, #5030, #16808, #19912, #8230, #15161, #3490, #15273, #18692, #1723, #11960, #11520, #9882, #21680, #1499, #4917, #6576, #6802, #173, #3593, #14821, #10320, #21788, #18250, #3150, #13294, #11630, #6905, #5136, #11853, #18359, #11739, #17022, #6457, #4798, #16698, #13611, #18583, #8337, #20244, #15049, #6695, #13402, #18472, #3375, #13511, #600, #2044, #15589, #14147, #12168, #9099, #5348, #18795, #10642, #392, #18901, #8775, #12278, #10426, #5666, #5551, #20670, #19014, #7120, #282, #10860, #8988, #13719, #3808, #20775, #7341, #7015, #17345, #10747, #19227, #20455, #13827, #12390, #19125, #4019, #2253, #17451, #3915, #4125, #15800, #20566, #3698, #14040, #12065, #15490 ),
 ( #12500, #15695, #20883, #5771, #2360, #5449, #710, #1932, #17130, #7443, #17233, #8665, #15387, #10535, #2149, #8882, #494, #7231, #13931, #16527, #2983, #13020, #6174, #9720, #7956, #19973, #6515, #14879, #16421, #7552, #13349, #1332, #1446, #14249, #16644, #21624, #14660, #13235, #4858, #815, #12908, #8174, #20994, #20086, #19630, #14986, #11577, #4523, #9828, #11245, #19851, #11461, #17558, #18305, #17966, #2871, #21731, #4633, #9614, #9938, #8066, #15904, #2465, #14772, #4741, #19741, #21403, #3208, #4973, #16313, #1554, #21515, #18189, #1223, #8285, #9205, #6400, #6639, #6289, #11353, #13128, #3097, #18075, #6926, #3509, #21699, #13423, #20262, #3284, #1628, #10233, #16934, #10124, #14953, #8579, #16829, #11874, #20160, #3398, #13632, #19936, #18493, #9800, #6820, #1742, #21808, #16493, #6599, #20053, #15296, #11650, #18271, #14844, #15185, #6717, #189, #20369, #8478, #87, #5265, #1412, #8139, #18711, #18385, #8361, #21589, #6480, #13317, #13200, #4821, #11545, #10014, #15072, #13528, #5050, #11761, #5155, #3175, #9904, #16608, #1522, #8251, #10771, #18929, #738, #17478, #12415, #413, #12300, #19144, #13954, #12086, #2273, #10556, #20584, #13740, #17258, #15511, #5691, #14065, #627, #2169 ),
 ( #18816, #7145, #3721, #3936, #20800, #7466, #10340, #14174, #8907, #7034, #20477, #5370, #10450, #2388, #7362, #4044, #17152, #15609, #20908, #5794, #12525, #2068, #9124, #15822, #3618, #15723, #17043, #8798, #1955, #8685, #15408, #306, #9012, #13849, #518, #5470, #12192, #3830, #7254, #20693, #19039, #5576, #10666, #17368, #7792, #5904, #1167, #1058, #16150, #14496, #17692, #17584, #6343, #4460, #9232, #7692, #16258, #17904, #2491, #12847, #6230, #14718, #15931, #9333, #7900, #14603, #21342, #19567, #12960, #21238, #21453, #11296, #2594, #21021, #2817, #7577, #10979, #10883, #16033, #842, #9555, #12634, #8010, #11192, #16364, #9664, #19684, #19355, #6117, #19250, #14276, #18018, #4153, #12740, #4253, #9450, #4575, #2929, #17796, #11082, #1276, #946, #14388, #21128, #6011, #19463, #4353, #2705, #13508, #20242, #13400, #18248, #5134, #20134, #15159, #16696, #6693, #10212, #1385, #21786, #13069, #10098, #5028, #9993, #19796, #3149, #1498, #11852, #8228, #21564, #18128, #18471, #1604, #59, #3487, #11737, #3374, #6801, #4687, #11404, #18581, #14930, #20030, #16915, #9775, #9880, #1827, #8560, #171, #16579, #21678, #16806, #6574, #13292, #1721, #15272, #4915, #3037, #16471, #8114, #11628, #8454 ) ),
 .UNSPECIFIED., .T., .F., .F. ) 
 B_SPLINE_SURFACE_WITH_KNOTS ( ( 4, 3, 4 ),
 ( 4, 2, 2, 2, 2, 2, 2, 2, 2, 2, 2, 2, 2, 2, 2, 2, 2, 2, 2, 2, 2, 2, 2, 2, 2, 2, 2, 2, 2, 2, 2, 2, 2, 2, 2, 2, 2, 2, 2, 2, 2, 2, 2, 2, 2, 2, 2, 2, 2, 2, 2, 2, 2, 2, 2, 2, 2, 2, 2, 2, 2, 2, 2, 2, 2, 2, 2, 2, 2, 2, 2, 2, 2, 2, 2, 2, 2, 2, 2, 2, 4 ),
 ( 0.000000000000000000, 0.5000000000000000000, 1.000000000000000000 ),
 ( 0.000000000000000000, 0.008318061648474830982, 0.01871563870907547167, 0.02911321576967611582, 0.03951079283027675998, 0.04990836989087740067, 0.06030594695147804829, 0.07070352401207868898, 0.08110110107267932966, 0.09149867813327997035, 0.1018962551938805972, 0.1122938322544812378, 0.1226914093150818785, 0.1330889863756825053, 0.1434865634362831321, 0.1538841404968837590, 0.1642817175574843858, 0.1746792946180850126, 0.1850768716786856394, 0.1954744487392862939, 0.2058720257998869485, 0.2162696028604875753, 0.2266671799210882021, 0.2370647569816888289, 0.2474623340422894557, 0.2578599111028900825, 0.2682574881634907094, 0.2786550652240913362, 0.2890526422846919630, 0.2994502193452925343, 0.3098477964058931611, 0.3202453734664937879, 0.3306429505270944147, 0.3410405275876950415, 0.3514381046482956683, 0.3618356817088962951, 0.3722332587694969219, 0.3826308358300975487, 0.3930284128906983421, 0.4034259899512990799, 0.4138235670118998732, 0.4242211440725006666, 0.4346187211331002942, 0.4450162981936999218, 0.4554138752542995494, 0.4658114523148991770, 0.4762090293755006920, 0.4866066064361021515, 0.4970041834967036110, 0.5074017605573051259, 0.5177993376179057528, 0.5281969146785063796, 0.5385944917391070064, 0.5489920687997077442, 0.5593896458603083710, 0.5697872229209089978, 0.5801847999815096246, 0.5905823770421102514, 0.6009799541027108782, 0.6113775311633115050, 0.6217751082239121319, 0.6321726852845127587, 0.6425702623451133855, 0.6529678394057140123, 0.6633654164663146391, 0.6737629935269152659, 0.6841605705875142274, 0.6945581476481130778, 0.7049557247087120393, 0.7153533017693110008, 0.7257508788299132929, 0.7361484558905155851, 0.7465460329511179882, 0.7569436100117202804, 0.7673411870723210182, 0.7777387641329216450, 0.7881363411935222718, 0.7985339182541228986, 0.8080132075800156022, 0.8174924969059083057, 0.8280181261579530050 ),
 .UNSPECIFIED. ) 
 GEOMETRIC_REPRESENTATION_ITEM ( )  RATIONAL_B_SPLINE_SURFACE ( (
 ( 1.000000000000000000, 1.000000000000000000, 1.000000000000000000, 1.000000000000000000, 1.000000000000000000, 1.000000000000000000, 1.000000000000000000, 1.000000000000000000, 1.000000000000000000, 1.000000000000000000, 1.000000000000000000, 1.000000000000000000, 1.000000000000000000, 1.000000000000000000, 1.000000000000000000, 1.000000000000000000, 1.000000000000000000, 1.000000000000000000, 1.000000000000000000, 1.000000000000000000, 1.000000000000000000, 1.000000000000000000, 1.000000000000000000, 1.000000000000000000, 1.000000000000000000, 1.000000000000000000, 1.000000000000000000, 1.000000000000000000, 1.000000000000000000, 1.000000000000000000, 1.000000000000000000, 1.000000000000000000, 1.000000000000000000, 1.000000000000000000, 1.000000000000000000, 1.000000000000000000, 1.000000000000000000, 1.000000000000000000, 1.000000000000000000, 1.000000000000000000, 1.000000000000000000, 1.000000000000000000, 1.000000000000000000, 1.000000000000000000, 1.000000000000000000, 1.000000000000000000, 1.000000000000000000, 1.000000000000000000, 1.000000000000000000, 1.000000000000000000, 1.000000000000000000, 1.000000000000000000, 1.000000000000000000, 1.000000000000000000, 1.000000000000000000, 1.000000000000000000, 1.000000000000000000, 1.000000000000000000, 1.000000000000000000, 1.000000000000000000, 1.000000000000000000, 1.000000000000000000, 1.000000000000000000, 1.000000000000000000, 1.000000000000000000, 1.000000000000000000, 1.000000000000000000, 1.000000000000000000, 1.000000000000000000, 1.000000000000000000, 1.000000000000000000, 1.000000000000000000, 1.000000000000000000, 1.000000000000000000, 1.000000000000000000, 1.000000000000000000, 1.000000000000000000, 1.000000000000000000, 1.000000000000000000, 1.000000000000000000, 1.000000000000000000, 1.000000000000000000, 1.000000000000000000, 1.000000000000000000, 1.000000000000000000, 1.000000000000000000, 1.000000000000000000, 1.000000000000000000, 1.000000000000000000, 1.000000000000000000, 1.000000000000000000, 1.000000000000000000, 1.000000000000000000, 1.000000000000000000, 1.000000000000000000, 1.000000000000000000, 1.000000000000000000, 1.000000000000000000, 1.000000000000000000, 1.000000000000000000, 1.000000000000000000, 1.000000000000000000, 1.000000000000000000, 1.000000000000000000, 1.000000000000000000, 1.000000000000000000, 1.000000000000000000, 1.000000000000000000, 1.000000000000000000, 1.000000000000000000, 1.000000000000000000, 1.000000000000000000, 1.000000000000000000, 1.000000000000000000, 1.000000000000000000, 1.000000000000000000, 1.000000000000000000, 1.000000000000000000, 1.000000000000000000, 1.000000000000000000, 1.000000000000000000, 1.000000000000000000, 1.000000000000000000, 1.000000000000000000, 1.000000000000000000, 1.000000000000000000, 1.000000000000000000, 1.000000000000000000, 1.000000000000000000, 1.000000000000000000, 1.000000000000000000, 1.000000000000000000, 1.000000000000000000, 1.000000000000000000, 1.000000000000000000, 1.000000000000000000, 1.000000000000000000, 1.000000000000000000, 1.000000000000000000, 1.000000000000000000, 1.000000000000000000, 1.000000000000000000, 1.000000000000000000, 1.000000000000000000, 1.000000000000000000, 1.000000000000000000, 1.000000000000000000, 1.000000000000000000, 1.000000000000000000, 1.000000000000000000, 1.000000000000000000, 1.000000000000000000, 1.000000000000000000, 1.000000000000000000, 1.000000000000000000, 1.000000000000000000, 1.000000000000000000, 1.000000000000000000, 1.000000000000000000, 1.000000000000000000, 1.000000000000000000, 1.000000000000000000),
 ( 0.3333333333333333703, 0.3333333333333333703, 0.3333333333333333703, 0.3333333333333333703, 0.3333333333333333703, 0.3333333333333333703, 0.3333333333333333703, 0.3333333333333333703, 0.3333333333333333703, 0.3333333333333333703, 0.3333333333333333703, 0.3333333333333333703, 0.3333333333333333703, 0.3333333333333333703, 0.3333333333333333703, 0.3333333333333333703, 0.3333333333333333703, 0.3333333333333333703, 0.3333333333333333703, 0.3333333333333333703, 0.3333333333333333703, 0.3333333333333333703, 0.3333333333333333703, 0.3333333333333333703, 0.3333333333333333703, 0.3333333333333333703, 0.3333333333333333703, 0.3333333333333333703, 0.3333333333333333703, 0.3333333333333333703, 0.3333333333333333703, 0.3333333333333333703, 0.3333333333333333703, 0.3333333333333333703, 0.3333333333333333703, 0.3333333333333333703, 0.3333333333333333703, 0.3333333333333333703, 0.3333333333333333703, 0.3333333333333333703, 0.3333333333333333703, 0.3333333333333333703, 0.3333333333333333703, 0.3333333333333333703, 0.3333333333333333703, 0.3333333333333333703, 0.3333333333333333703, 0.3333333333333333703, 0.3333333333333333703, 0.3333333333333333703, 0.3333333333333333703, 0.3333333333333333703, 0.3333333333333333703, 0.3333333333333333703, 0.3333333333333333703, 0.3333333333333333703, 0.3333333333333333703, 0.3333333333333333703, 0.3333333333333333703, 0.3333333333333333703, 0.3333333333333333703, 0.3333333333333333703, 0.3333333333333333703, 0.3333333333333333703, 0.3333333333333333703, 0.3333333333333333703, 0.3333333333333333703, 0.3333333333333333703, 0.3333333333333333703, 0.3333333333333333703, 0.3333333333333333703, 0.3333333333333333703, 0.3333333333333333703, 0.3333333333333333703, 0.3333333333333333703, 0.3333333333333333703, 0.3333333333333333703, 0.3333333333333333703, 0.3333333333333333703, 0.3333333333333333703, 0.3333333333333333703, 0.3333333333333333703, 0.3333333333333333703, 0.3333333333333333703, 0.3333333333333333703, 0.3333333333333333703, 0.3333333333333333703, 0.3333333333333333703, 0.3333333333333333703, 0.3333333333333333703, 0.3333333333333333703, 0.3333333333333333703, 0.3333333333333333703, 0.3333333333333333703, 0.3333333333333333703, 0.3333333333333333703, 0.3333333333333333703, 0.3333333333333333703, 0.3333333333333333703, 0.3333333333333333703, 0.3333333333333333703, 0.3333333333333333703, 0.3333333333333333703, 0.3333333333333333703, 0.3333333333333333703, 0.3333333333333333703, 0.3333333333333333703, 0.3333333333333333703, 0.3333333333333333703, 0.3333333333333333703, 0.3333333333333333703, 0.3333333333333333703, 0.3333333333333333703, 0.3333333333333333703, 0.3333333333333333703, 0.3333333333333333703, 0.3333333333333333703, 0.3333333333333333703, 0.3333333333333333703, 0.3333333333333333703, 0.3333333333333333703, 0.3333333333333333703, 0.3333333333333333703, 0.3333333333333333703, 0.3333333333333333703, 0.3333333333333333703, 0.3333333333333333703, 0.3333333333333333703, 0.3333333333333333703, 0.3333333333333333703, 0.3333333333333333703, 0.3333333333333333703, 0.3333333333333333703, 0.3333333333333333703, 0.3333333333333333703, 0.3333333333333333703, 0.3333333333333333703, 0.3333333333333333703, 0.3333333333333333703, 0.3333333333333333703, 0.3333333333333333703, 0.3333333333333333703, 0.3333333333333333703, 0.3333333333333333703, 0.3333333333333333703, 0.3333333333333333703, 0.3333333333333333703, 0.3333333333333333703, 0.3333333333333333703, 0.3333333333333333703, 0.3333333333333333703, 0.3333333333333333703, 0.3333333333333333703, 0.3333333333333333703, 0.3333333333333333703, 0.3333333333333333703, 0.3333333333333333703, 0.3333333333333333703, 0.3333333333333333703, 0.3333333333333333703, 0.3333333333333333703, 0.3333333333333333703),
 ( 0.3333333333333333703, 0.3333333333333333703, 0.3333333333333333703, 0.3333333333333333703, 0.3333333333333333703, 0.3333333333333333703, 0.3333333333333333703, 0.3333333333333333703, 0.3333333333333333703, 0.3333333333333333703, 0.3333333333333333703, 0.3333333333333333703, 0.3333333333333333703, 0.3333333333333333703, 0.3333333333333333703, 0.3333333333333333703, 0.3333333333333333703, 0.3333333333333333703, 0.3333333333333333703, 0.3333333333333333703, 0.3333333333333333703, 0.3333333333333333703, 0.3333333333333333703, 0.3333333333333333703, 0.3333333333333333703, 0.3333333333333333703, 0.3333333333333333703, 0.3333333333333333703, 0.3333333333333333703, 0.3333333333333333703, 0.3333333333333333703, 0.3333333333333333703, 0.3333333333333333703, 0.3333333333333333703, 0.3333333333333333703, 0.3333333333333333703, 0.3333333333333333703, 0.3333333333333333703, 0.3333333333333333703, 0.3333333333333333703, 0.3333333333333333703, 0.3333333333333333703, 0.3333333333333333703, 0.3333333333333333703, 0.3333333333333333703, 0.3333333333333333703, 0.3333333333333333703, 0.3333333333333333703, 0.3333333333333333703, 0.3333333333333333703, 0.3333333333333333703, 0.3333333333333333703, 0.3333333333333333703, 0.3333333333333333703, 0.3333333333333333703, 0.3333333333333333703, 0.3333333333333333703, 0.3333333333333333703, 0.3333333333333333703, 0.3333333333333333703, 0.3333333333333333703, 0.3333333333333333703, 0.3333333333333333703, 0.3333333333333333703, 0.3333333333333333703, 0.3333333333333333703, 0.3333333333333333703, 0.3333333333333333703, 0.3333333333333333703, 0.3333333333333333703, 0.3333333333333333703, 0.3333333333333333703, 0.3333333333333333703, 0.3333333333333333703, 0.3333333333333333703, 0.3333333333333333703, 0.3333333333333333703, 0.3333333333333333703, 0.3333333333333333703, 0.3333333333333333703, 0.3333333333333333703, 0.3333333333333333703, 0.3333333333333333703, 0.3333333333333333703, 0.3333333333333333703, 0.3333333333333333703, 0.3333333333333333703, 0.3333333333333333703, 0.3333333333333333703, 0.3333333333333333703, 0.3333333333333333703, 0.3333333333333333703, 0.3333333333333333703, 0.3333333333333333703, 0.3333333333333333703, 0.3333333333333333703, 0.3333333333333333703, 0.3333333333333333703, 0.3333333333333333703, 0.3333333333333333703, 0.3333333333333333703, 0.3333333333333333703, 0.3333333333333333703, 0.3333333333333333703, 0.3333333333333333703, 0.3333333333333333703, 0.3333333333333333703, 0.3333333333333333703, 0.3333333333333333703, 0.3333333333333333703, 0.3333333333333333703, 0.3333333333333333703, 0.3333333333333333703, 0.3333333333333333703, 0.3333333333333333703, 0.3333333333333333703, 0.3333333333333333703, 0.3333333333333333703, 0.3333333333333333703, 0.3333333333333333703, 0.3333333333333333703, 0.3333333333333333703, 0.3333333333333333703, 0.3333333333333333703, 0.3333333333333333703, 0.3333333333333333703, 0.3333333333333333703, 0.3333333333333333703, 0.3333333333333333703, 0.3333333333333333703, 0.3333333333333333703, 0.3333333333333333703, 0.3333333333333333703, 0.3333333333333333703, 0.3333333333333333703, 0.3333333333333333703, 0.3333333333333333703, 0.3333333333333333703, 0.3333333333333333703, 0.3333333333333333703, 0.3333333333333333703, 0.3333333333333333703, 0.3333333333333333703, 0.3333333333333333703, 0.3333333333333333703, 0.3333333333333333703, 0.3333333333333333703, 0.3333333333333333703, 0.3333333333333333703, 0.3333333333333333703, 0.3333333333333333703, 0.3333333333333333703, 0.3333333333333333703, 0.3333333333333333703, 0.3333333333333333703, 0.3333333333333333703, 0.3333333333333333703, 0.3333333333333333703, 0.3333333333333333703, 0.3333333333333333703, 0.3333333333333333703, 0.3333333333333333703),
 ( 1.000000000000000000, 1.000000000000000000, 1.000000000000000000, 1.000000000000000000, 1.000000000000000000, 1.000000000000000000, 1.000000000000000000, 1.000000000000000000, 1.000000000000000000, 1.000000000000000000, 1.000000000000000000, 1.000000000000000000, 1.000000000000000000, 1.000000000000000000, 1.000000000000000000, 1.000000000000000000, 1.000000000000000000, 1.000000000000000000, 1.000000000000000000, 1.000000000000000000, 1.000000000000000000, 1.000000000000000000, 1.000000000000000000, 1.000000000000000000, 1.000000000000000000, 1.000000000000000000, 1.000000000000000000, 1.000000000000000000, 1.000000000000000000, 1.000000000000000000, 1.000000000000000000, 1.000000000000000000, 1.000000000000000000, 1.000000000000000000, 1.000000000000000000, 1.000000000000000000, 1.000000000000000000, 1.000000000000000000, 1.000000000000000000, 1.000000000000000000, 1.000000000000000000, 1.000000000000000000, 1.000000000000000000, 1.000000000000000000, 1.000000000000000000, 1.000000000000000000, 1.000000000000000000, 1.000000000000000000, 1.000000000000000000, 1.000000000000000000, 1.000000000000000000, 1.000000000000000000, 1.000000000000000000, 1.000000000000000000, 1.000000000000000000, 1.000000000000000000, 1.000000000000000000, 1.000000000000000000, 1.000000000000000000, 1.000000000000000000, 1.000000000000000000, 1.000000000000000000, 1.000000000000000000, 1.000000000000000000, 1.000000000000000000, 1.000000000000000000, 1.000000000000000000, 1.000000000000000000, 1.000000000000000000, 1.000000000000000000, 1.000000000000000000, 1.000000000000000000, 1.000000000000000000, 1.000000000000000000, 1.000000000000000000, 1.000000000000000000, 1.000000000000000000, 1.000000000000000000, 1.000000000000000000, 1.000000000000000000, 1.000000000000000000, 1.000000000000000000, 1.000000000000000000, 1.000000000000000000, 1.000000000000000000, 1.000000000000000000, 1.000000000000000000, 1.000000000000000000, 1.000000000000000000, 1.000000000000000000, 1.000000000000000000, 1.000000000000000000, 1.000000000000000000, 1.000000000000000000, 1.000000000000000000, 1.000000000000000000, 1.000000000000000000, 1.000000000000000000, 1.000000000000000000, 1.000000000000000000, 1.000000000000000000, 1.000000000000000000, 1.000000000000000000, 1.000000000000000000, 1.000000000000000000, 1.000000000000000000, 1.000000000000000000, 1.000000000000000000, 1.000000000000000000, 1.000000000000000000, 1.000000000000000000, 1.000000000000000000, 1.000000000000000000, 1.000000000000000000, 1.000000000000000000, 1.000000000000000000, 1.000000000000000000, 1.000000000000000000, 1.000000000000000000, 1.000000000000000000, 1.000000000000000000, 1.000000000000000000, 1.000000000000000000, 1.000000000000000000, 1.000000000000000000, 1.000000000000000000, 1.000000000000000000, 1.000000000000000000, 1.000000000000000000, 1.000000000000000000, 1.000000000000000000, 1.000000000000000000, 1.000000000000000000, 1.000000000000000000, 1.000000000000000000, 1.000000000000000000, 1.000000000000000000, 1.000000000000000000, 1.000000000000000000, 1.000000000000000000, 1.000000000000000000, 1.000000000000000000, 1.000000000000000000, 1.000000000000000000, 1.000000000000000000, 1.000000000000000000, 1.000000000000000000, 1.000000000000000000, 1.000000000000000000, 1.000000000000000000, 1.000000000000000000, 1.000000000000000000, 1.000000000000000000, 1.000000000000000000, 1.000000000000000000, 1.000000000000000000, 1.000000000000000000, 1.000000000000000000, 1.000000000000000000, 1.000000000000000000, 1.000000000000000000, 1.000000000000000000),
 ( 0.3333333333333333703, 0.3333333333333333703, 0.3333333333333333703, 0.3333333333333333703, 0.3333333333333333703, 0.3333333333333333703, 0.3333333333333333703, 0.3333333333333333703, 0.3333333333333333703, 0.3333333333333333703, 0.3333333333333333703, 0.3333333333333333703, 0.3333333333333333703, 0.3333333333333333703, 0.3333333333333333703, 0.3333333333333333703, 0.3333333333333333703, 0.3333333333333333703, 0.3333333333333333703, 0.3333333333333333703, 0.3333333333333333703, 0.3333333333333333703, 0.3333333333333333703, 0.3333333333333333703, 0.3333333333333333703, 0.3333333333333333703, 0.3333333333333333703, 0.3333333333333333703, 0.3333333333333333703, 0.3333333333333333703, 0.3333333333333333703, 0.3333333333333333703, 0.3333333333333333703, 0.3333333333333333703, 0.3333333333333333703, 0.3333333333333333703, 0.3333333333333333703, 0.3333333333333333703, 0.3333333333333333703, 0.3333333333333333703, 0.3333333333333333703, 0.3333333333333333703, 0.3333333333333333703, 0.3333333333333333703, 0.3333333333333333703, 0.3333333333333333703, 0.3333333333333333703, 0.3333333333333333703, 0.3333333333333333703, 0.3333333333333333703, 0.3333333333333333703, 0.3333333333333333703, 0.3333333333333333703, 0.3333333333333333703, 0.3333333333333333703, 0.3333333333333333703, 0.3333333333333333703, 0.3333333333333333703, 0.3333333333333333703, 0.3333333333333333703, 0.3333333333333333703, 0.3333333333333333703, 0.3333333333333333703, 0.3333333333333333703, 0.3333333333333333703, 0.3333333333333333703, 0.3333333333333333703, 0.3333333333333333703, 0.3333333333333333703, 0.3333333333333333703, 0.3333333333333333703, 0.3333333333333333703, 0.3333333333333333703, 0.3333333333333333703, 0.3333333333333333703, 0.3333333333333333703, 0.3333333333333333703, 0.3333333333333333703, 0.3333333333333333703, 0.3333333333333333703, 0.3333333333333333703, 0.3333333333333333703, 0.3333333333333333703, 0.3333333333333333703, 0.3333333333333333703, 0.3333333333333333703, 0.3333333333333333703, 0.3333333333333333703, 0.3333333333333333703, 0.3333333333333333703, 0.3333333333333333703, 0.3333333333333333703, 0.3333333333333333703, 0.3333333333333333703, 0.3333333333333333703, 0.3333333333333333703, 0.3333333333333333703, 0.3333333333333333703, 0.3333333333333333703, 0.3333333333333333703, 0.3333333333333333703, 0.3333333333333333703, 0.3333333333333333703, 0.3333333333333333703, 0.3333333333333333703, 0.3333333333333333703, 0.3333333333333333703, 0.3333333333333333703, 0.3333333333333333703, 0.3333333333333333703, 0.3333333333333333703, 0.3333333333333333703, 0.3333333333333333703, 0.3333333333333333703, 0.3333333333333333703, 0.3333333333333333703, 0.3333333333333333703, 0.3333333333333333703, 0.3333333333333333703, 0.3333333333333333703, 0.3333333333333333703, 0.3333333333333333703, 0.3333333333333333703, 0.3333333333333333703, 0.3333333333333333703, 0.3333333333333333703, 0.3333333333333333703, 0.3333333333333333703, 0.3333333333333333703, 0.3333333333333333703, 0.3333333333333333703, 0.3333333333333333703, 0.3333333333333333703, 0.3333333333333333703, 0.3333333333333333703, 0.3333333333333333703, 0.3333333333333333703, 0.3333333333333333703, 0.3333333333333333703, 0.3333333333333333703, 0.3333333333333333703, 0.3333333333333333703, 0.3333333333333333703, 0.3333333333333333703, 0.3333333333333333703, 0.3333333333333333703, 0.3333333333333333703, 0.3333333333333333703, 0.3333333333333333703, 0.3333333333333333703, 0.3333333333333333703, 0.3333333333333333703, 0.3333333333333333703, 0.3333333333333333703, 0.3333333333333333703, 0.3333333333333333703, 0.3333333333333333703, 0.3333333333333333703, 0.3333333333333333703, 0.3333333333333333703, 0.3333333333333333703, 0.3333333333333333703),
 ( 0.3333333333333333703, 0.3333333333333333703, 0.3333333333333333703, 0.3333333333333333703, 0.3333333333333333703, 0.3333333333333333703, 0.3333333333333333703, 0.3333333333333333703, 0.3333333333333333703, 0.3333333333333333703, 0.3333333333333333703, 0.3333333333333333703, 0.3333333333333333703, 0.3333333333333333703, 0.3333333333333333703, 0.3333333333333333703, 0.3333333333333333703, 0.3333333333333333703, 0.3333333333333333703, 0.3333333333333333703, 0.3333333333333333703, 0.3333333333333333703, 0.3333333333333333703, 0.3333333333333333703, 0.3333333333333333703, 0.3333333333333333703, 0.3333333333333333703, 0.3333333333333333703, 0.3333333333333333703, 0.3333333333333333703, 0.3333333333333333703, 0.3333333333333333703, 0.3333333333333333703, 0.3333333333333333703, 0.3333333333333333703, 0.3333333333333333703, 0.3333333333333333703, 0.3333333333333333703, 0.3333333333333333703, 0.3333333333333333703, 0.3333333333333333703, 0.3333333333333333703, 0.3333333333333333703, 0.3333333333333333703, 0.3333333333333333703, 0.3333333333333333703, 0.3333333333333333703, 0.3333333333333333703, 0.3333333333333333703, 0.3333333333333333703, 0.3333333333333333703, 0.3333333333333333703, 0.3333333333333333703, 0.3333333333333333703, 0.3333333333333333703, 0.3333333333333333703, 0.3333333333333333703, 0.3333333333333333703, 0.3333333333333333703, 0.3333333333333333703, 0.3333333333333333703, 0.3333333333333333703, 0.3333333333333333703, 0.3333333333333333703, 0.3333333333333333703, 0.3333333333333333703, 0.3333333333333333703, 0.3333333333333333703, 0.3333333333333333703, 0.3333333333333333703, 0.3333333333333333703, 0.3333333333333333703, 0.3333333333333333703, 0.3333333333333333703, 0.3333333333333333703, 0.3333333333333333703, 0.3333333333333333703, 0.3333333333333333703, 0.3333333333333333703, 0.3333333333333333703, 0.3333333333333333703, 0.3333333333333333703, 0.3333333333333333703, 0.3333333333333333703, 0.3333333333333333703, 0.3333333333333333703, 0.3333333333333333703, 0.3333333333333333703, 0.3333333333333333703, 0.3333333333333333703, 0.3333333333333333703, 0.3333333333333333703, 0.3333333333333333703, 0.3333333333333333703, 0.3333333333333333703, 0.3333333333333333703, 0.3333333333333333703, 0.3333333333333333703, 0.3333333333333333703, 0.3333333333333333703, 0.3333333333333333703, 0.3333333333333333703, 0.3333333333333333703, 0.3333333333333333703, 0.3333333333333333703, 0.3333333333333333703, 0.3333333333333333703, 0.3333333333333333703, 0.3333333333333333703, 0.3333333333333333703, 0.3333333333333333703, 0.3333333333333333703, 0.3333333333333333703, 0.3333333333333333703, 0.3333333333333333703, 0.3333333333333333703, 0.3333333333333333703, 0.3333333333333333703, 0.3333333333333333703, 0.3333333333333333703, 0.3333333333333333703, 0.3333333333333333703, 0.3333333333333333703, 0.3333333333333333703, 0.3333333333333333703, 0.3333333333333333703, 0.3333333333333333703, 0.3333333333333333703, 0.3333333333333333703, 0.3333333333333333703, 0.3333333333333333703, 0.3333333333333333703, 0.3333333333333333703, 0.3333333333333333703, 0.3333333333333333703, 0.3333333333333333703, 0.3333333333333333703, 0.3333333333333333703, 0.3333333333333333703, 0.3333333333333333703, 0.3333333333333333703, 0.3333333333333333703, 0.3333333333333333703, 0.3333333333333333703, 0.3333333333333333703, 0.3333333333333333703, 0.3333333333333333703, 0.3333333333333333703, 0.3333333333333333703, 0.3333333333333333703, 0.3333333333333333703, 0.3333333333333333703, 0.3333333333333333703, 0.3333333333333333703, 0.3333333333333333703, 0.3333333333333333703, 0.3333333333333333703, 0.3333333333333333703, 0.3333333333333333703, 0.3333333333333333703, 0.3333333333333333703, 0.3333333333333333703),
 ( 1.000000000000000000, 1.000000000000000000, 1.000000000000000000, 1.000000000000000000, 1.000000000000000000, 1.000000000000000000, 1.000000000000000000, 1.000000000000000000, 1.000000000000000000, 1.000000000000000000, 1.000000000000000000, 1.000000000000000000, 1.000000000000000000, 1.000000000000000000, 1.000000000000000000, 1.000000000000000000, 1.000000000000000000, 1.000000000000000000, 1.000000000000000000, 1.000000000000000000, 1.000000000000000000, 1.000000000000000000, 1.000000000000000000, 1.000000000000000000, 1.000000000000000000, 1.000000000000000000, 1.000000000000000000, 1.000000000000000000, 1.000000000000000000, 1.000000000000000000, 1.000000000000000000, 1.000000000000000000, 1.000000000000000000, 1.000000000000000000, 1.000000000000000000, 1.000000000000000000, 1.000000000000000000, 1.000000000000000000, 1.000000000000000000, 1.000000000000000000, 1.000000000000000000, 1.000000000000000000, 1.000000000000000000, 1.000000000000000000, 1.000000000000000000, 1.000000000000000000, 1.000000000000000000, 1.000000000000000000, 1.000000000000000000, 1.000000000000000000, 1.000000000000000000, 1.000000000000000000, 1.000000000000000000, 1.000000000000000000, 1.000000000000000000, 1.000000000000000000, 1.000000000000000000, 1.000000000000000000, 1.000000000000000000, 1.000000000000000000, 1.000000000000000000, 1.000000000000000000, 1.000000000000000000, 1.000000000000000000, 1.000000000000000000, 1.000000000000000000, 1.000000000000000000, 1.000000000000000000, 1.000000000000000000, 1.000000000000000000, 1.000000000000000000, 1.000000000000000000, 1.000000000000000000, 1.000000000000000000, 1.000000000000000000, 1.000000000000000000, 1.000000000000000000, 1.000000000000000000, 1.000000000000000000, 1.000000000000000000, 1.000000000000000000, 1.000000000000000000, 1.000000000000000000, 1.000000000000000000, 1.000000000000000000, 1.000000000000000000, 1.000000000000000000, 1.000000000000000000, 1.000000000000000000, 1.000000000000000000, 1.000000000000000000, 1.000000000000000000, 1.000000000000000000, 1.000000000000000000, 1.000000000000000000, 1.000000000000000000, 1.000000000000000000, 1.000000000000000000, 1.000000000000000000, 1.000000000000000000, 1.000000000000000000, 1.000000000000000000, 1.000000000000000000, 1.000000000000000000, 1.000000000000000000, 1.000000000000000000, 1.000000000000000000, 1.000000000000000000, 1.000000000000000000, 1.000000000000000000, 1.000000000000000000, 1.000000000000000000, 1.000000000000000000, 1.000000000000000000, 1.000000000000000000, 1.000000000000000000, 1.000000000000000000, 1.000000000000000000, 1.000000000000000000, 1.000000000000000000, 1.000000000000000000, 1.000000000000000000, 1.000000000000000000, 1.000000000000000000, 1.000000000000000000, 1.000000000000000000, 1.000000000000000000, 1.000000000000000000, 1.000000000000000000, 1.000000000000000000, 1.000000000000000000, 1.000000000000000000, 1.000000000000000000, 1.000000000000000000, 1.000000000000000000, 1.000000000000000000, 1.000000000000000000, 1.000000000000000000, 1.000000000000000000, 1.000000000000000000, 1.000000000000000000, 1.000000000000000000, 1.000000000000000000, 1.000000000000000000, 1.000000000000000000, 1.000000000000000000, 1.000000000000000000, 1.000000000000000000, 1.000000000000000000, 1.000000000000000000, 1.000000000000000000, 1.000000000000000000, 1.000000000000000000, 1.000000000000000000, 1.000000000000000000, 1.000000000000000000, 1.000000000000000000, 1.000000000000000000, 1.000000000000000000, 1.000000000000000000, 1.000000000000000000, 1.000000000000000000) ) ) 
 REPRESENTATION_ITEM ( '' )  SURFACE ( )  );
#14596 = CARTESIAN_POINT ( 'NONE',  ( 43.06284635655732274, 148.1064719378950088, -10.08176808973812655 ) ) ;
#14597 = CARTESIAN_POINT ( 'NONE',  ( -145.6429501568359797, -185.9438272943107506, 41.63779006702063867 ) ) ;
#14598 = CARTESIAN_POINT ( 'NONE',  ( 38.58424406990785371, 96.26518717409400949, 35.64915139335015937 ) ) ;
#14599 = EDGE_CURVE ( 'NONE', #13513, #6293, #7412, .T. ) ;
#14600 = DIRECTION ( 'NONE',  ( 0.000000000000000000, 0.000000000000000000, 1.000000000000000000 ) ) ;
#14601 = VERTEX_POINT ( 'NONE', #4861 ) ;
#14602 = DIRECTION ( 'NONE',  ( 1.000000000000000000, 0.000000000000000000, -1.140132994654635861E-16 ) ) ;
#14603 = CARTESIAN_POINT ( 'NONE',  ( 40.02721236285810136, 85.80382532021769748, 0.4343372985580923329 ) ) ;
#14604 = CARTESIAN_POINT ( 'NONE',  ( 22.52008984372607614, 139.2495111981779985, 17.01435058386764965 ) ) ;
#14605 = CARTESIAN_POINT ( 'NONE',  ( 41.64333658814960870, 63.97977050742731109, 38.42115945441014446 ) ) ;
#14606 = ORIENTED_EDGE ( 'NONE', *, *, #9756, .F. ) ;
#14607 = VERTEX_POINT ( 'NONE', #18424 ) ;
#14608 = CARTESIAN_POINT ( 'NONE',  ( 45.74753988029933538, 155.3297705074273267, 30.44471234641811819 ) ) ;
#14609 = EDGE_CURVE ( 'NONE', #14883, #2955, #9665, .T. ) ;
#14610 = CYLINDRICAL_SURFACE ( 'NONE', #19674, 10.00000000000000888 ) ;
#14611 = CIRCLE ( 'NONE', #1601, 10.00000000000000888 ) ;
#14612 = EDGE_CURVE ( 'NONE', #3209, #14572, #16394, .T. ) ;
#14613 = CARTESIAN_POINT ( 'NONE',  ( 41.46631938032478359, 114.1104996726487428, 29.45539723777780239 ) ) ;
#14614 = CARTESIAN_POINT ( 'NONE',  ( 45.74753988029933538, 71.06518717409400665, 30.44471234641811819 ) ) ;
#14615 = CARTESIAN_POINT ( 'NONE',  ( 41.46631938032478359, 65.18445800887258201, 29.45539723777780239 ) ) ;
#14616 = CARTESIAN_POINT ( 'NONE',  ( -159.0959885057557983, -175.5938272943107279, 55.19815736654470584 ) ) ;
#14617 = CARTESIAN_POINT ( 'NONE',  ( 43.01140435219951286, 152.0344580088725763, 29.21067981925356705 ) ) ;
#14618 = CARTESIAN_POINT ( 'NONE',  ( -145.2889157411863721, -179.6130981290892805, 41.15050349809590102 ) ) ;
#14619 = CARTESIAN_POINT ( 'NONE',  ( 43.01140435219951996, 10.71049967264875491, 34.21067981925357060 ) ) ;
#14620 = CARTESIAN_POINT ( 'NONE',  ( 39.92123440845004723, 153.2344580088725934, 38.46393386101376421 ) ) ;
#14621 = CARTESIAN_POINT ( 'NONE',  ( 46.59305225739526435, 130.5797705074273267, 36.81289934271958941 ) ) ;
#14622 = CARTESIAN_POINT ( 'NONE',  ( 43.13803657676253067, 85.59359249887060628, 13.33475322466254198 ) ) ;
#14623 = CARTESIAN_POINT ( 'NONE',  ( 45.74753988029934249, 128.0651871740940067, 30.44471234641812174 ) ) ;
#14624 = CARTESIAN_POINT ( 'NONE',  ( 43.01140435219957681, 68.96049967264870872, 29.21067981925356705 ) ) ;
#14625 = DIRECTION ( 'NONE',  ( -0.000000000000000000, -0.000000000000000000, 1.000000000000000000 ) ) ;
#14626 = CARTESIAN_POINT ( 'NONE',  ( 68.01140435219951996, 119.9070776186055838, 50.00000000000002842 ) ) ;
#14627 = CARTESIAN_POINT ( 'NONE',  ( 46.10157429594899270, 149.6604996726486831, 29.95742577749336988 ) ) ;
#14628 = CARTESIAN_POINT ( 'NONE',  ( 70.35668680342836012, 113.0167181193761508, -8.057780719902234878 ) ) ;
#14629 = AXIS2_PLACEMENT_3D ( 'NONE', #20733, #15651, #3657 ) ;
#14630 = CARTESIAN_POINT ( 'NONE',  ( 47.05648932407426344, 83.51049967264874851, 31.27175355779120025 ) ) ;
#14631 = VERTEX_POINT ( 'NONE', #6518 ) ;
#14632 = SHAPE_REPRESENTATION ( 'Handle Balance Tension Spring', ( #12657 ), #19020 ) ;
#14633 = DIRECTION ( 'NONE',  ( 1.000000000000000000, 0.000000000000000000, -1.734723475976805615E-16 ) ) ;
#14634 = ORIENTED_EDGE ( 'NONE', *, *, #9508, .F. ) ;
#14635 = CARTESIAN_POINT ( 'NONE',  ( 39.92123440845004723, 81.23445800887256496, 38.46393386101376421 ) ) ;
#14636 = CARTESIAN_POINT ( 'NONE',  ( 43.80332655382220253, 102.6113394311928317, 39.21067981925355639 ) ) ;
#14637 = CARTESIAN_POINT ( 'NONE',  ( 43.01140435219951286, 139.4604996726487514, 39.46799094044489209 ) ) ;
#14639 = CARTESIAN_POINT ( 'NONE',  ( 39.14927582833848874, 92.05416703502255871, 8.565614722876343734 ) ) ;
#14638 = CARTESIAN_POINT ( 'NONE',  ( 43.01140435219951286, 96.86518717409398960, 38.86567161673127657 ) ) ;
#14640 = CARTESIAN_POINT ( 'NONE',  ( -154.3824083646099439, -164.7584106276440536, 40.69124936498395328 ) ) ;
#14641 = CARTESIAN_POINT ( 'NONE',  ( 38.01140435219951996, 60.86049967264872862, 35.83527830041810347 ) ) ;
#14643 = CARTESIAN_POINT ( 'NONE',  ( 44.55648932407425633, 69.68445800887256780, 38.96596240072933170 ) ) ;
#14642 = CARTESIAN_POINT ( 'NONE',  ( 18.67254549292281141, -61.68114226949890622, -46.21320343559645494 ) ) ;
#14644 = CARTESIAN_POINT ( 'NONE',  ( 39.92123440845005433, 106.1604996726487400, 38.46393386101375711 ) ) ;
#14645 = VECTOR ( 'NONE', #8812, 1000.000000000000114 ) ;
#14646 = CYLINDRICAL_SURFACE ( 'NONE', #19168, 15.54735917280169311 ) ;
#14647 = DIRECTION ( 'NONE',  ( -1.000000000000000000, -0.000000000000000000, -0.000000000000000000 ) ) ;
#14648 = AXIS2_PLACEMENT_3D ( 'NONE', #6782, #7100, #21767 ) ;
#14649 = CARTESIAN_POINT ( 'NONE',  ( 44.37947211624943833, 157.2797705074273438, 38.42115945441014446 ) ) ;
#14650 = CARTESIAN_POINT ( 'NONE',  ( 134.3985507411545939, 186.9327686461008682, 21.73429951086134082 ) ) ;
#14651 = CARTESIAN_POINT ( 'NONE',  ( 39.42975644700377558, 150.4151871740940010, 36.81289934271958941 ) ) ;
#14652 = CYLINDRICAL_SURFACE ( 'NONE', #19434, 4.999999999999997335 ) ;
#14653 = CARTESIAN_POINT ( 'NONE',  ( -160.8964159109769696, -169.8938272943107393, 49.65701158161630957 ) ) ;
#14654 = CARTESIAN_POINT ( 'NONE',  ( -157.2955611005345986, -181.7084106276440423, 57.67623309621197336 ) ) ;
#14655 = VERTEX_POINT ( 'NONE', #13239 ) ;
#14656 = CARTESIAN_POINT ( 'NONE',  ( 46.59305225739526435, 67.31518717409400665, 36.81289934271958941 ) ) ;
#14657 = CARTESIAN_POINT ( 'NONE',  ( -145.6429501568359797, -165.2084106276440423, 41.63779006702063867 ) ) ;
#14658 = CARTESIAN_POINT ( 'NONE',  ( 14.54084317601859588, 100.7536435603138756, 21.43002817983359876 ) ) ;
#14659 = CARTESIAN_POINT ( 'NONE',  ( 43.01140435219951286, 138.8651871740940180, 38.86567161673127657 ) ) ;
#14660 = CARTESIAN_POINT ( 'NONE',  ( 9.046145050308979307, 123.4917717844193277, -10.79923121120670437 ) ) ;
#14661 = AXIS2_PLACEMENT_3D ( 'NONE', #18203, #15118, #9953 ) ;
#14662 = ORIENTED_EDGE ( 'NONE', *, *, #11740, .T. ) ;
#14663 = VERTEX_POINT ( 'NONE', #6751 ) ;
#14664 = ADVANCED_FACE ( 'NONE', ( #3211 ), #5085, .F. ) ;
#14665 = CARTESIAN_POINT ( 'NONE',  ( 20.99626426110969390, 137.5292218135913913, 9.918250401459649979 ) ) ;
#14666 = AXIS2_PLACEMENT_3D ( 'NONE', #19229, #12392, #19127 ) ;
#14667 = ORIENTED_EDGE ( 'NONE', *, *, #16951, .F. ) ;
#14668 = CARTESIAN_POINT ( 'NONE',  ( 43.80332655382220253, 116.8836182503284817, 29.21067981925356705 ) ) ;
#14669 = CARTESIAN_POINT ( 'NONE',  ( 43.01140435219951286, 76.12977050742732388, 38.86567161673127657 ) ) ;
#14671 = CARTESIAN_POINT ( 'NONE',  ( 15.96294818963569639, 111.9339314265907745, 8.846935114401974332 ) ) ;
#14670 = CARTESIAN_POINT ( 'NONE',  ( 38.58424406990784661, 125.9651871740939697, 32.77220824515698183 ) ) ;
#14672 = CARTESIAN_POINT ( 'NONE',  ( 41.46631938032478359, 94.31049967264874567, 38.96596240072933170 ) ) ;
#14673 = CARTESIAN_POINT ( 'NONE',  ( 76.66991938639012005, 113.6622739410785670, 5.791450954060403333 ) ) ;
#14674 = FACE_OUTER_BOUND ( 'NONE', #14283, .T. ) ;
#14675 = CARTESIAN_POINT ( 'NONE',  ( -148.3790856849358306, -159.3891397928654783, 40.14644641866477315 ) ) ;
#14676 = CARTESIAN_POINT ( 'NONE',  ( 47.43856463449117200, 91.46518717409398391, 35.64915139335016647 ) ) ;
#14677 = AXIS2_PLACEMENT_3D ( 'NONE', #14642, #2853, #12779 ) ;
#14678 = CARTESIAN_POINT ( 'NONE',  ( 44.55648932407425633, 107.8104996726487457, 29.45539723777780239 ) ) ;
#14679 = CARTESIAN_POINT ( 'NONE',  ( 43.01140435219951286, 86.03445800887256212, 29.21067981925356705 ) ) ;
#14680 = CARTESIAN_POINT ( 'NONE',  ( 48.01140435219951996, 142.2844580088725763, 34.21067981925357060 ) ) ;
#14681 = ORIENTED_EDGE ( 'NONE', *, *, #7908, .T. ) ;
#14682 = CARTESIAN_POINT ( 'NONE',  ( 45.74753988029933538, 77.32977050742729830, 30.44471234641811819 ) ) ;
#14683 = CARTESIAN_POINT ( 'NONE',  ( -148.5561028927606344, -192.0584106276440650, 40.69124936498395328 ) ) ;
#14684 = CARTESIAN_POINT ( 'NONE',  ( 57.78275410301085913, 89.02518083909171764, -0.1607367497116551913 ) ) ;
#14685 = CARTESIAN_POINT ( 'NONE',  ( -143.8425227516148084, -183.3584106276440480, 44.11586579668791330 ) ) ;
#14686 = ORIENTED_EDGE ( 'NONE', *, *, #10598, .F. ) ;
#14687 = CARTESIAN_POINT ( 'NONE',  ( 40.27526882409969033, 158.6651871740939725, 30.44471234641811819 ) ) ;
#14688 = LINE ( 'NONE', #11490, #3599 ) ;
#14689 = CARTESIAN_POINT ( 'NONE',  ( 43.01140435219951286, 127.1297705074273097, 38.86567161673127657 ) ) ;
#14690 = VECTOR ( 'NONE', #781, 1000.000000000000114 ) ;
#14691 = EDGE_LOOP ( 'NONE', ( #17097, #15771, #13587, #195 ) ) ;
#14692 = DIRECTION ( 'NONE',  ( -0.000000000000000000, -0.000000000000000000, -1.000000000000000000 ) ) ;
#14693 = ORIENTED_EDGE ( 'NONE', *, *, #17399, .T. ) ;
#14694 = AXIS2_PLACEMENT_3D ( 'NONE', #5232, #10306, #7216 ) ;
#14695 = DIRECTION ( 'NONE',  ( 0.000000000000000000, 0.000000000000000000, -1.000000000000000000 ) ) ;
#14696 = CARTESIAN_POINT ( 'NONE',  ( 41.64333658814960870, 87.97977050742731819, 38.42115945441014446 ) ) ;
#14697 = CARTESIAN_POINT ( 'NONE',  ( 43.01140435219951286, 62.03445800887257633, 28.95336869806222779 ) ) ;
#14698 = EDGE_CURVE ( 'NONE', #12353, #1800, #20922, .T. ) ;
#14699 = CYLINDRICAL_SURFACE ( 'NONE', #6958, 44.28464465043163756 ) ;
#14700 = CARTESIAN_POINT ( 'NONE',  ( 41.46631938032478359, 101.1844580088725678, 29.45539723777780239 ) ) ;
#14701 = CARTESIAN_POINT ( 'NONE',  ( -161.4692556286852891, -176.6391397928654783, 46.40781461928724383 ) ) ;
#14702 = CARTESIAN_POINT ( 'NONE',  ( -141.4692556286852891, -189.8391397928654953, 46.40781461928724383 ) ) ;
#14703 = VECTOR ( 'NONE', #6254, 1000.000000000000114 ) ;
#14704 = CARTESIAN_POINT ( 'NONE',  ( 111.4021762516569964, 137.5714195593754710, 272.0939500981630204 ) ) ;
#14705 = CARTESIAN_POINT ( 'NONE',  ( 53.01140435219953417, 119.9070776186055838, -19.99999999999998579 ) ) ;
#14706 = PRODUCT_DEFINITION ( 'UNKNOWN', '', #10218, #4652 ) ;
#14707 = CARTESIAN_POINT ( 'NONE',  ( -160.8964159109769696, -194.0438272943107165, 46.59394152635518793 ) ) ;
#14708 = ITEM_DEFINED_TRANSFORMATION ( 'NONE', 'NONE', #1063,  #12657 ) ;
#14709 = CARTESIAN_POINT ( 'NONE',  ( 41.46631938032478359, 126.3844580088725706, 38.96596240072933170 ) ) ;
#14710 = CARTESIAN_POINT ( 'NONE',  ( 44.37947211624943833, 103.2797705074273154, 38.42115945441014446 ) ) ;
#14711 = CARTESIAN_POINT ( 'NONE',  ( 16.54882264740998110, 129.8072851447780067, 22.56993813403257931 ) ) ;
#14712 = CARTESIAN_POINT ( 'NONE',  ( -159.0959885057557983, -182.1938272943107506, 44.11586579668791330 ) ) ;
#14713 = CARTESIAN_POINT ( 'NONE',  ( 46.59305225739526435, 88.31518717409400665, 36.81289934271958941 ) ) ;
#14714 = FACE_OUTER_BOUND ( 'NONE', #7463, .T. ) ;
#14715 = ORIENTED_EDGE ( 'NONE', *, *, #7470, .F. ) ;
#14716 = FACE_OUTER_BOUND ( 'NONE', #20666, .T. ) ;
#14717 = ADVANCED_FACE ( 'NONE', ( #17290 ), #7502, .T. ) ;
#14718 = CARTESIAN_POINT ( 'NONE',  ( 61.01612483116806374, 90.79174121657607088, -0.2798613066081144796 ) ) ;
#14719 = CARTESIAN_POINT ( 'NONE',  ( 60.58642193167724344, 97.95666160567475345, -13.33918631239395225 ) ) ;
#14720 = CARTESIAN_POINT ( 'NONE',  ( 38.58424406990786082, 63.37977050742732388, 34.21067981925357060 ) ) ;
#14721 = ORIENTED_EDGE ( 'NONE', *, *, #9655, .F. ) ;
#14722 = EDGE_CURVE ( 'NONE', #12379, #1227, #13771, .T. ) ;
#14723 = ORIENTED_EDGE ( 'NONE', *, *, #268, .F. ) ;
#14724 = CARTESIAN_POINT ( 'NONE',  ( 41.64333658814960870, 156.9797705074273040, 38.42115945441014446 ) ) ;
#14725 = DIRECTION ( 'NONE',  ( -0.000000000000000000, -0.000000000000000000, -1.000000000000000000 ) ) ;
#14726 = CARTESIAN_POINT ( 'NONE',  ( 48.01140435219951996, 107.2104996726487371, 34.21067981925357060 ) ) ;
#14727 = CARTESIAN_POINT ( 'NONE',  ( 41.64333658814960870, 72.71518717409399812, 38.42115945441014446 ) ) ;
#14728 = CARTESIAN_POINT ( 'NONE',  ( 38.01140435219952707, 65.93445800887258201, 35.83527830041809636 ) ) ;
#14729 =( BOUNDED_CURVE ( )  B_SPLINE_CURVE ( 2, ( #7454, #14481, #5890, #21225, #7350, #17571, #14054, #2374, #19133, #10757, #12620, #15811, #7564 ),
 .UNSPECIFIED., .F., .F. ) 
 B_SPLINE_CURVE_WITH_KNOTS ( ( 3, 2, 2, 2, 2, 2, 3 ),
 ( 0.2426470588235294101, 0.2441176470588235226, 0.2470588235294117752, 0.2500000000000000000, 0.2529411764705882248, 0.2558823529411764497, 0.2573529411764705621 ),
 .UNSPECIFIED. ) 
 CURVE ( )  GEOMETRIC_REPRESENTATION_ITEM ( )  RATIONAL_B_SPLINE_CURVE ( ( 0.9755282581475768211, 0.9755282581475768211, 1.000000000000000000, 0.9510565162951535312, 1.000000000000000000, 0.9510565162951535312, 1.000000000000000000, 0.9510565162951535312, 1.000000000000000000, 0.9510565162951535312, 1.000000000000000000, 0.9755282581475772652, 0.9755282581475768211 ) ) 
 REPRESENTATION_ITEM ( '' )  );
#14730 = CARTESIAN_POINT ( 'NONE',  ( -143.8425227516148084, -162.0938272943107279, 44.11586579668791330 ) ) ;
#14731 = CARTESIAN_POINT ( 'NONE',  ( 43.01140435219951996, 2.710499672648754466, 59.21067981925355639 ) ) ;
#14732 = CARTESIAN_POINT ( 'NONE',  ( -161.4692556286852607, -181.4130981290892919, 52.90620854394536821 ) ) ;
#14733 =( LENGTH_UNIT ( ) NAMED_UNIT ( * ) SI_UNIT ( .MILLI., .METRE. ) );
#14734 = CARTESIAN_POINT ( 'NONE',  ( 44.55648932407425633, 148.8844580088725991, 29.45539723777780239 ) ) ;
#14735 = CARTESIAN_POINT ( 'NONE',  ( 40.27526882409969033, 129.8297705074273267, 37.97664729208901946 ) ) ;
#14736 = CARTESIAN_POINT ( 'NONE',  ( 30.67228459367742133, 151.9265198579663263, 16.42994147312239051 ) ) ;
#14737 = CARTESIAN_POINT ( 'NONE',  ( 47.43856463449118621, 124.6151871740940038, 34.21067981925357060 ) ) ;
#14738 = DIRECTION ( 'NONE',  ( -0.000000000000000000, -0.000000000000000000, -1.000000000000000000 ) ) ;
#14739 = CARTESIAN_POINT ( 'NONE',  ( -143.8425227516148084, -159.9584106276440423, 55.19815736654470584 ) ) ;
#14740 = ADVANCED_FACE ( 'NONE', ( #18847 ), #8721, .F. ) ;
#14741 = CARTESIAN_POINT ( 'NONE',  ( 43.01140435219951286, 64.46049967264873715, 39.21067981925356349 ) ) ;
#14742 = DIRECTION ( 'NONE',  ( -0.3450121214752274179, 0.9385982292947088190, -0.000000000000000000 ) ) ;
#14743 = CARTESIAN_POINT ( 'NONE',  ( 67.11143925497957241, 134.7062941969633414, 18.05698923925237764 ) ) ;
#14744 = LINE ( 'NONE', #12877, #10761 ) ;
#14745 = AXIS2_PLACEMENT_3D ( 'NONE', #9483, #17833, #2744 ) ;
#14746 = VERTEX_POINT ( 'NONE', #15439 ) ;
#14747 = ORIENTED_EDGE ( 'NONE', *, *, #660, .T. ) ;
#14748 = CARTESIAN_POINT ( 'NONE',  ( 147.5268905834513475, 193.0332408774651185, 14.00000000000001776 ) ) ;
#14749 = CARTESIAN_POINT ( 'NONE',  ( 41.46631938032478359, 139.3104996726487457, 38.96596240072933170 ) ) ;
#14751 = CARTESIAN_POINT ( 'NONE',  ( 70.48507635059884535, 125.9029633330538189, 6.422671151982867421 ) ) ;
#14750 = CARTESIAN_POINT ( 'NONE',  ( 41.64333658814960870, 99.71518717409399812, 38.42115945441014446 ) ) ;
#14752 = CARTESIAN_POINT ( 'NONE',  ( -148.5561028927606344, -171.0584106276440366, 40.69124936498395328 ) ) ;
#14753 = CARTESIAN_POINT ( 'NONE',  ( -160.8964159109769696, -194.0438272943107165, 46.59394152635518083 ) ) ;
#14755 = CARTESIAN_POINT ( 'NONE',  ( 43.01140435219951996, 10.71049967264875491, 39.21067981925356349 ) ) ;
#14754 = CARTESIAN_POINT ( 'NONE',  ( -153.0531000319306827, -179.2362167067689995, 39.65701158161629536 ) ) ;
#14756 = CARTESIAN_POINT ( 'NONE',  ( -148.3790856849358306, -189.6630981290893203, 59.16757674456786020 ) ) ;
#14757 = PRESENTATION_LAYER_ASSIGNMENT (  '', '', ( #1042 ) ) ;
#14758 = CARTESIAN_POINT ( 'NONE',  ( 43.80332655382220253, 115.9575765865522925, 29.21067981925356705 ) ) ;
#14759 = CARTESIAN_POINT ( 'NONE',  ( 46.59305225739526435, 157.5797705074273267, 36.81289934271958941 ) ) ;
#14760 = DIRECTION ( 'NONE',  ( 1.723963091245776585E-16, 6.336983651701956765E-17, 1.000000000000000000 ) ) ;
#14761 = CARTESIAN_POINT ( 'NONE',  ( 42.92180000979148957, 85.67454126555050209, 7.339147150375312734 ) ) ;
#14762 = CARTESIAN_POINT ( 'NONE',  ( -157.2955611005346270, -161.3438272943107563, 41.63779006702063867 ) ) ;
#14763 = CARTESIAN_POINT ( 'NONE',  ( -143.8425227516148084, -183.3584106276440480, 44.11586579668791330 ) ) ;
#14764 = ADVANCED_FACE ( 'NONE', ( #1988 ), #19069, .T. ) ;
#14765 = EDGE_CURVE ( 'NONE', #4022, #8340, #3613, .T. ) ;
#14766 = ORIENTED_EDGE ( 'NONE', *, *, #4303, .T. ) ;
#14767 = CARTESIAN_POINT ( 'NONE',  ( 46.59305225739526435, 73.91518717409400097, 31.60846029578754468 ) ) ;
#14768 = CARTESIAN_POINT ( 'NONE',  ( -143.8425227516148084, -174.3584106276440480, 44.11586579668791330 ) ) ;
#14769 = CARTESIAN_POINT ( 'NONE',  ( 75.73800832010900308, 109.5907576069244698, 18.92991194937467014 ) ) ;
#14770 = CARTESIAN_POINT ( 'NONE',  ( 43.01140435219951286, 113.0344580088725763, 29.21067981925356705 ) ) ;
#14771 = CARTESIAN_POINT ( 'NONE',  ( 39.42975644700377558, 131.8151871740940067, 31.60846029578754468 ) ) ;
#14772 = CARTESIAN_POINT ( 'NONE',  ( 50.69626032627856915, 86.62977272806217854, -5.918438612465169335 ) ) ;
#14773 = ORIENTED_EDGE ( 'NONE', *, *, #7909, .F. ) ;
#14774 = ORIENTED_EDGE ( 'NONE', *, *, #1256, .F. ) ;
#14775 = CARTESIAN_POINT ( 'NONE',  ( -148.5561028927606344, -166.2584106276440536, 58.62277379824867296 ) ) ;
#14776 = CARTESIAN_POINT ( 'NONE',  ( 17.98614708603287937, 106.9092867359673704, 15.63253669370310384 ) ) ;
#14777 = VERTEX_POINT ( 'NONE', #17401 ) ;
#14778 = CARTESIAN_POINT ( 'NONE',  ( 43.01140435219957681, 93.53445800887259054, 39.21067981925356349 ) ) ;
#14779 = CARTESIAN_POINT ( 'NONE',  ( 38.58424406990784661, 63.22977050742731109, 32.77220824515698183 ) ) ;
#14781 = CARTESIAN_POINT ( 'NONE',  ( 24.77189431714078083, 141.4131305960171687, 3.132649400142189844 ) ) ;
#14780 = CARTESIAN_POINT ( 'NONE',  ( 46.59305225739526435, 127.9151871740940010, 31.60846029578754468 ) ) ;
#14782 = CARTESIAN_POINT ( 'NONE',  ( 38.01140435219952707, 93.71049967264875136, 34.21067981925357060 ) ) ;
#14783 = PLANE ( 'NONE',  #4417 ) ;
#14784 = CARTESIAN_POINT ( 'NONE',  ( -141.4692556286852891, -170.9130981290893203, 46.40781461928724383 ) ) ;
#14785 = CARTESIAN_POINT ( 'NONE',  ( 41.46631938032478359, 138.1104996726487286, 29.45539723777780239 ) ) ;
#14786 = CARTESIAN_POINT ( 'NONE',  ( 41.64333658814960870, 86.51518717409399528, 30.00020018409699318 ) ) ;
#14787 = CARTESIAN_POINT ( 'NONE',  ( -120.0322075325610598, -136.9891397928655010, -54.65701158161630246 ) ) ;
#14788 = CARTESIAN_POINT ( 'NONE',  ( -151.4692556286852891, -196.9891397928655010, 49.65701158161630957 ) ) ;
#14789 = VECTOR ( 'NONE', #3537, 1000.000000000000000 ) ;
#14790 = EDGE_LOOP ( 'NONE', ( #21395, #17613, #15457, #1904 ) ) ;
#14791 = CARTESIAN_POINT ( 'NONE',  ( 46.59305225739526435, 77.17977050742732104, 31.60846029578754468 ) ) ;
#14792 = CARTESIAN_POINT ( 'NONE',  ( -142.0420953463935803, -156.2438272943106767, 46.59394152635518793 ) ) ;
#14793 = CARTESIAN_POINT ( 'NONE',  ( 34.41316853928974950, 153.0433231119815503, 10.55326060710041958 ) ) ;
#14794 = CARTESIAN_POINT ( 'NONE',  ( -145.6429501568359797, -181.1084106276440195, 57.67623309621198047 ) ) ;
#14795 = ORIENTED_EDGE ( 'NONE', *, *, #9467, .F. ) ;
#14796 = CARTESIAN_POINT ( 'NONE',  ( 165.8083469658213005, 192.9029763258799335, -44.99999999999997158 ) ) ;
#14797 = CARTESIAN_POINT ( 'NONE',  ( -151.4692556286852891, -196.9891397928655010, 59.65701158161632378 ) ) ;
#14798 = CARTESIAN_POINT ( 'NONE',  ( 38.58424406990786082, 126.3797705074273239, 34.21067981925357060 ) ) ;
#14799 = ORIENTED_EDGE ( 'NONE', *, *, #4767, .F. ) ;
#14800 = CARTESIAN_POINT ( 'NONE',  ( 47.05648932407426344, 129.9844580088725934, 37.14960608071593384 ) ) ;
#14801 = ORIENTED_EDGE ( 'NONE', *, *, #3391, .F. ) ;
#14802 = CARTESIAN_POINT ( 'NONE',  ( 45.74753988029933538, 119.3297705074273267, 30.44471234641811819 ) ) ;
#14803 = STYLED_ITEM ( 'NONE', ( #334 ), #353 ) ;
#14804 = CARTESIAN_POINT ( 'NONE',  ( 39.42975644700377558, 87.07977050742732672, 31.60846029578754468 ) ) ;
#14805 = CARTESIAN_POINT ( 'NONE',  ( 47.43856463449118621, 151.6151871740939896, 34.21067981925357060 ) ) ;
#14806 = CYLINDRICAL_SURFACE ( 'NONE', #21377, 7.500000000000007105 ) ;
#14807 = LINE ( 'NONE', #12945, #7491 ) ;
#14808 = SURFACE_STYLE_FILL_AREA ( #21438 ) ;
#14809 = CARTESIAN_POINT ( 'NONE',  ( -143.3790856849358306, -184.2891397928654840, 55.53486410454105027 ) ) ;
#14810 = DIRECTION ( 'NONE',  ( 0.000000000000000000, 1.000000000000000000, 0.000000000000000000 ) ) ;
#14811 = CARTESIAN_POINT ( 'NONE',  ( -157.2955611005346270, -187.4438272943106938, 57.67623309621198047 ) ) ;
#14812 = CARTESIAN_POINT ( 'NONE',  ( 43.01140435219951286, 125.0344580088725763, 28.95336869806222779 ) ) ;
#14813 = CARTESIAN_POINT ( 'NONE',  ( 39.42975644700377558, 105.6797705074273352, 36.81289934271958941 ) ) ;
#14814 = CARTESIAN_POINT ( 'NONE',  ( 19.91114674846567922, 103.5922903064164302, 14.48528786281536895 ) ) ;
#14815 = CARTESIAN_POINT ( 'NONE',  ( -145.6429501568359797, -179.9438272943107506, 41.63779006702063867 ) ) ;
#14816 = CARTESIAN_POINT ( 'NONE',  ( 38.58424406990785371, 90.26518717409398107, 35.64915139335015937 ) ) ;
#14817 = DIRECTION ( 'NONE',  ( 0.000000000000000000, 1.000000000000000000, 0.000000000000000000 ) ) ;
#14818 = ORIENTED_EDGE ( 'NONE', *, *, #21480, .F. ) ;
#14819 = DIRECTION ( 'NONE',  ( 0.000000000000000000, 0.000000000000000000, 1.000000000000000000 ) ) ;
#14820 = FACE_OUTER_BOUND ( 'NONE', #8121, .T. ) ;
#14821 = CARTESIAN_POINT ( 'NONE',  ( 68.32201692705490359, 132.1587870917933003, -0.8393580998851425390 ) ) ;
#14822 = CARTESIAN_POINT ( 'NONE',  ( 44.37947211624943833, 62.47977050742731109, 30.00020018409699318 ) ) ;
#14823 = VERTEX_POINT ( 'NONE', #17183 ) ;
#14824 = EDGE_LOOP ( 'NONE', ( #17348, #15438, #17640, #13176 ) ) ;
#14825 = CARTESIAN_POINT ( 'NONE',  ( 45.74753988029933538, 143.3297705074272699, 30.44471234641811819 ) ) ;
#14826 = ADVANCED_FACE ( 'NONE', ( #15754 ), #2303, .F. ) ;
#14827 = DIRECTION ( 'NONE',  ( -0.000000000000000000, -0.000000000000000000, 1.000000000000000000 ) ) ;
#14828 = CARTESIAN_POINT ( 'NONE',  ( 46.10157429594899270, 109.7604996726487485, 38.46393386101376421 ) ) ;
#14829 = CARTESIAN_POINT ( 'NONE',  ( 39.42975644700377558, 72.41518717409400097, 36.81289934271958941 ) ) ;
#14830 = CARTESIAN_POINT ( 'NONE',  ( -151.4692556286852891, -195.9891397928654726, 49.65701158161630957 ) ) ;
#14831 = CARTESIAN_POINT ( 'NONE',  ( -154.3824083646099439, -158.4938272943107052, 40.69124936498395328 ) ) ;
#14832 = CARTESIAN_POINT ( 'NONE',  ( -148.3790856849358306, -166.5891397928654669, 59.16757674456786020 ) ) ;
#14833 = CARTESIAN_POINT ( 'NONE',  ( -154.5594255724347761, -179.1630981290893203, 40.14644641866476604 ) ) ;
#14834 = DIRECTION ( 'NONE',  ( -0.000000000000000000, 1.000000000000000000, -0.000000000000000000 ) ) ;
#14835 = CARTESIAN_POINT ( 'NONE',  ( 46.10157429594899270, 147.8344580088725309, 38.46393386101376421 ) ) ;
#14836 = CARTESIAN_POINT ( 'NONE',  ( 40.27526882409969033, 135.8297705074273551, 37.97664729208901946 ) ) ;
#14837 = CARTESIAN_POINT ( 'NONE',  ( 70.19659433329162823, 140.8466096914638399, 17.85851290171837746 ) ) ;
#14838 = CARTESIAN_POINT ( 'NONE',  ( 44.37947211624943833, 119.2151871740939981, 30.00020018409699318 ) ) ;
#14839 = CARTESIAN_POINT ( 'NONE',  ( -154.5594255724347761, -181.8891397928654783, 59.16757674456785310 ) ) ;
#14840 = VECTOR ( 'NONE', #14625, 1000.000000000000000 ) ;
#14841 = PLANE ( 'NONE',  #770 ) ;
#14843 = LINE ( 'NONE', #12873, #21407 ) ;
#14842 = AXIS2_PLACEMENT_3D ( 'NONE', #21538, #4768, #16446 ) ;
#14844 = CARTESIAN_POINT ( 'NONE',  ( 10.18435502709129103, 110.4832086711448227, 2.772112504659519416 ) ) ;
#14845 = CARTESIAN_POINT ( 'NONE',  ( 23.45520590541277883, 99.47716203340817742, 21.27102736060455257 ) ) ;
#14846 = CARTESIAN_POINT ( 'NONE',  ( -145.2889157411863437, -187.4391397928654612, 58.16351966513671812 ) ) ;
#14847 = CIRCLE ( 'NONE', #4643, 7.500000000000000000 ) ;
#14848 = CARTESIAN_POINT ( 'NONE',  ( 44.37947211624943833, 98.47977050742731819, 30.00020018409699318 ) ) ;
#14849 = ORIENTED_EDGE ( 'NONE', *, *, #20210, .F. ) ;
#14850 = CARTESIAN_POINT ( 'NONE',  ( -141.4692556286852891, -168.2130981290892748, 52.90620854394536821 ) ) ;
#14851 = ORIENTED_EDGE ( 'NONE', *, *, #12435, .F. ) ;
#14852 =( BOUNDED_CURVE ( )  B_SPLINE_CURVE ( 2, ( #2139, #15264, #15579, #15150, #3365, #10089, #18680, #16797, #6893, #1710, #20232, #20444, #3479 ),
 .UNSPECIFIED., .F., .F. ) 
 B_SPLINE_CURVE_WITH_KNOTS ( ( 3, 2, 2, 2, 2, 2, 3 ),
 ( 0.5808823529411765163, 0.5823529411764706287, 0.5852941176470588536, 0.5882352941176470784, 0.5911764705882353033, 0.5941176470588235281, 0.5955882352941176405 ),
 .UNSPECIFIED. ) 
 CURVE ( )  GEOMETRIC_REPRESENTATION_ITEM ( )  RATIONAL_B_SPLINE_CURVE ( ( 0.9755282581475768211, 0.9755282581475768211, 1.000000000000000000, 0.9510565162951535312, 1.000000000000000000, 0.9510565162951535312, 1.000000000000000000, 0.9510565162951535312, 1.000000000000000000, 0.9510565162951535312, 1.000000000000000000, 0.9755282581475768211, 0.9755282581475768211 ) ) 
 REPRESENTATION_ITEM ( '' )  );
#14853 = CARTESIAN_POINT ( 'NONE',  ( 38.01140435219951996, 83.93445800887258201, 35.83527830041810347 ) ) ;
#14854 = CARTESIAN_POINT ( 'NONE',  ( 46.10157429594899270, 102.8344580088725877, 38.46393386101375711 ) ) ;
#14855 = CARTESIAN_POINT ( 'NONE',  ( 38.01140435219951996, 141.8604996726487286, 35.83527830041810347 ) ) ;
#14857 = CARTESIAN_POINT ( 'NONE',  ( 17.95776995827587896, 107.1383635228311846, 9.636927859708212196 ) ) ;
#14856 = CARTESIAN_POINT ( 'NONE',  ( 45.74753988029933538, 97.16518717409398675, 37.97664729208901946 ) ) ;
#14858 = CARTESIAN_POINT ( 'NONE',  ( -142.0420953463935803, -171.8084106276440366, 52.72008163687743831 ) ) ;
#14859 = CARTESIAN_POINT ( 'NONE',  ( -142.0420953463935803, -195.2438272943107336, 46.59394152635518083 ) ) ;
#14861 = DIRECTION ( 'NONE',  ( -1.000000000000000000, 0.000000000000000000, 0.000000000000000000 ) ) ;
#14860 = CARTESIAN_POINT ( 'NONE',  ( -159.5594255724347761, -166.2630981290893146, 55.53486410454104316 ) ) ;
#14862 = DIRECTION ( 'NONE',  ( -0.8624407588727071028, 0.5061580162706792452, 0.000000000000000000 ) ) ;
#14863 = EDGE_CURVE ( 'NONE', #10856, #13802, #5824, .T. ) ;
#14864 = LINE ( 'NONE', #16408, #15284 ) ;
#14865 = CARTESIAN_POINT ( 'NONE',  ( 39.92123440845005433, 78.26049967264873430, 29.95742577749336988 ) ) ;
#14866 = CARTESIAN_POINT ( 'NONE',  ( 39.42975644700377558, 156.6797705074273210, 36.81289934271958941 ) ) ;
#14867 = CARTESIAN_POINT ( 'NONE',  ( -154.5594255724347761, -185.1630981290893203, 40.14644641866476604 ) ) ;
#14868 = ADVANCED_FACE ( 'NONE', ( #3648 ), #8934, .T. ) ;
#14869 = CARTESIAN_POINT ( 'NONE',  ( 58.57487293839693621, 150.3975950434478648, 4.362879525569486994 ) ) ;
#14870 = CARTESIAN_POINT ( 'NONE',  ( 38.58424406990785371, 143.9651871740940123, 32.77220824515697473 ) ) ;
#14871 = CARTESIAN_POINT ( 'NONE',  ( -142.0420953463935803, -162.5438272943106881, 52.72008163687743831 ) ) ;
#14872 = CARTESIAN_POINT ( 'NONE',  ( -142.0420953463935803, -183.8084106276440082, 52.72008163687743831 ) ) ;
#14873 = EDGE_LOOP ( 'NONE', ( #9996, #2461, #14111, #6723 ) ) ;
#14874 = CARTESIAN_POINT ( 'NONE',  ( 40.27526882409969744, 68.66518717409400097, 30.44471234641812174 ) ) ;
#14875 = CARTESIAN_POINT ( 'NONE',  ( -142.0420953463935803, -171.8084106276440366, 52.72008163687743831 ) ) ;
#14876 = CARTESIAN_POINT ( 'NONE',  ( 62.21295035458982881, 148.3457431455455549, 17.50134052088148096 ) ) ;
#14877 = FACE_OUTER_BOUND ( 'NONE', #5875, .T. ) ;
#14878 = CARTESIAN_POINT ( 'NONE',  ( 41.64333658814960870, 128.5151871740939953, 30.00020018409699318 ) ) ;
#14879 = CARTESIAN_POINT ( 'NONE',  ( 33.37504612857446773, 87.14074678364892179, -12.34672919366563981 ) ) ;
#14880 = VERTEX_POINT ( 'NONE', #13878 ) ;
#14881 = ORIENTED_EDGE ( 'NONE', *, *, #3444, .F. ) ;
#14882 = CARTESIAN_POINT ( 'NONE',  ( -143.3790856849358306, -192.6891397928654897, 43.77915905869157598 ) ) ;
#14883 = VERTEX_POINT ( 'NONE', #20617 ) ;
#14884 = CARTESIAN_POINT ( 'NONE',  ( 47.05648932407426344, 109.5844580088725735, 31.27175355779120025 ) ) ;
#14885 = CARTESIAN_POINT ( 'NONE',  ( 43.01140435219951996, 10.71049967264875491, 34.21067981925357060 ) ) ;
#14886 = CARTESIAN_POINT ( 'NONE',  ( 47.43856463449118621, 64.87977050742730967, 34.21067981925357060 ) ) ;
#14888 = CARTESIAN_POINT ( 'NONE',  ( 14.93692188586762803, 117.2531131035273546, 2.061388125607503952 ) ) ;
#14887 = CARTESIAN_POINT ( 'NONE',  ( 44.37947211624943833, 124.0151871740939953, 38.42115945441014446 ) ) ;
#14889 = CARTESIAN_POINT ( 'NONE',  ( 48.01140435219951996, 83.06049967264873146, 35.83527830041810347 ) ) ;
#14890 = DIRECTION ( 'NONE',  ( -0.000000000000000000, -0.000000000000000000, 1.000000000000000000 ) ) ;
#14891 = CARTESIAN_POINT ( 'NONE',  ( 41.46631938032478359, 145.3104996726487457, 38.96596240072933170 ) ) ;
#14892 = DIRECTION ( 'NONE',  ( 0.000000000000000000, -1.000000000000000000, 0.000000000000000000 ) ) ;
#14893 = CARTESIAN_POINT ( 'NONE',  ( 39.42975644700377558, 92.81518717409399244, 31.60846029578754468 ) ) ;
#14894 = CARTESIAN_POINT ( 'NONE',  ( 47.05648932407426344, 151.5844580088725877, 31.27175355779120025 ) ) ;
#14895 = CARTESIAN_POINT ( 'NONE',  ( 43.01140435219951286, 62.96049967264873004, 29.21067981925356705 ) ) ;
#14896 = ORIENTED_EDGE ( 'NONE', *, *, #18208, .T. ) ;
#14897 = CARTESIAN_POINT ( 'NONE',  ( 38.58424406990784661, 66.22977050742728977, 32.77220824515698183 ) ) ;
#14898 = CARTESIAN_POINT ( 'NONE',  ( -160.8964159109769696, -157.8938272943107393, 49.65701158161630957 ) ) ;
#14899 = CARTESIAN_POINT ( 'NONE',  ( 37.24990543953586553, 153.6521207556136517, 3.648881909465930828 ) ) ;
#14900 = CARTESIAN_POINT ( 'NONE',  ( -142.0420953463935803, -183.5084106276440252, 46.59394152635518793 ) ) ;
#14901 = ORIENTED_EDGE ( 'NONE', *, *, #8548, .F. ) ;
#14902 = CARTESIAN_POINT ( 'NONE',  ( 47.43856463449117200, 157.7651871740939953, 32.77220824515698183 ) ) ;
#14903 = CARTESIAN_POINT ( 'NONE',  ( -143.3790856849358306, -160.2891397928654555, 55.53486410454105027 ) ) ;
#14904 = CARTESIAN_POINT ( 'NONE',  ( 46.59305225739526435, 113.1797705074273210, 31.60846029578754468 ) ) ;
#14905 = CARTESIAN_POINT ( 'NONE',  ( 64.11693453485118255, 146.8606268255622638, -2.422805558527139080 ) ) ;
#14906 = ORIENTED_EDGE ( 'NONE', *, *, #11365, .T. ) ;
#14907 = CARTESIAN_POINT ( 'NONE',  ( 47.05648932407426344, 130.5844580088725877, 31.27175355779120025 ) ) ;
#14908 = VERTEX_POINT ( 'NONE', #12230 ) ;
#14909 = CARTESIAN_POINT ( 'NONE',  ( 46.59305225739526435, 121.5797705074273267, 36.81289934271958941 ) ) ;
#14910 = PLANE ( 'NONE',  #12178 ) ;
#14911 = CARTESIAN_POINT ( 'NONE',  ( 39.42975644700377558, 155.8151871740940067, 31.60846029578754468 ) ) ;
#14912 = CARTESIAN_POINT ( 'NONE',  ( 12.59043673732666946, 104.3826120832696773, 9.557940159192295226 ) ) ;
#14913 = CARTESIAN_POINT ( 'NONE',  ( 43.01140435219951286, 74.03445800887257633, 29.21067981925356705 ) ) ;
#14914 = FACE_OUTER_BOUND ( 'NONE', #12639, .T. ) ;
#14915 = LINE ( 'NONE', #3358, #429 ) ;
#14916 = CARTESIAN_POINT ( 'NONE',  ( -143.3790856849358306, -177.6891397928654612, 43.77915905869157598 ) ) ;
#14917 = DIRECTION ( 'NONE',  ( -0.000000000000000000, -0.000000000000000000, -1.000000000000000000 ) ) ;
#14918 = CARTESIAN_POINT ( 'NONE',  ( 48.01140435219951996, 131.2104996726487514, 34.21067981925357060 ) ) ;
#14919 = CARTESIAN_POINT ( 'NONE',  ( -148.5561028927606344, -191.7938272943107449, 40.69124936498395328 ) ) ;
#14920 = PRODUCT_CONTEXT ( 'NONE', #19855, 'mechanical' ) ;
#14921 = CARTESIAN_POINT ( 'NONE',  ( 39.92123440845004723, 125.3344580088725735, 29.95742577749337343 ) ) ;
#14922 = CARTESIAN_POINT ( 'NONE',  ( 47.43856463449117200, 97.72977050742730398, 35.64915139335016647 ) ) ;
#14923 = CARTESIAN_POINT ( 'NONE',  ( 32.78705717043479240, 146.2756902729748560, 16.50925200294354056 ) ) ;
#14924 = CARTESIAN_POINT ( 'NONE',  ( -157.2955611005346270, -182.3438272943106995, 41.63779006702063867 ) ) ;
#14925 = CARTESIAN_POINT ( 'NONE',  ( 43.01140435219951286, 92.36518717409398960, 29.55568802177586107 ) ) ;
#14926 = CARTESIAN_POINT ( 'NONE',  ( 42.21948215057684450, 90.03738109496902098, 29.21067981925356705 ) ) ;
#14927 = VERTEX_POINT ( 'NONE', #3862 ) ;
#14928 = CARTESIAN_POINT ( 'NONE',  ( 43.01140435219951996, 10.71049967264875491, 34.21067981925357060 ) ) ;
#14929 = CIRCLE ( 'NONE', #15304, 3.000000000000050626 ) ;
#14930 = CARTESIAN_POINT ( 'NONE',  ( 53.04203944364535772, 87.17698241397053494, 14.00585298808814194 ) ) ;
#14931 = CARTESIAN_POINT ( 'NONE',  ( 44.37947211624943833, 140.4797705074273324, 30.00020018409699318 ) ) ;
#14932 = CARTESIAN_POINT ( 'NONE',  ( 46.34060549886174840, 91.98545359010019240, -5.720099531362743406 ) ) ;
#14933 = CARTESIAN_POINT ( 'NONE',  ( 41.64333658814960870, 65.77977050742732956, 30.00020018409699318 ) ) ;
#14934 = ORIENTED_EDGE ( 'NONE', *, *, #192, .F. ) ;
#14935 = CARTESIAN_POINT ( 'NONE',  ( 46.59305225739526435, 146.1797705074273495, 31.60846029578754468 ) ) ;
#14936 = ADVANCED_FACE ( 'NONE', ( #15640 ), #1091, .T. ) ;
#14937 = CARTESIAN_POINT ( 'NONE',  ( 47.43856463449117200, 97.72977050742730398, 35.64915139335016647 ) ) ;
#14938 = VECTOR ( 'NONE', #3275, 1000.000000000000000 ) ;
#14939 = CARTESIAN_POINT ( 'NONE',  ( 38.96631938032478359, 115.0104996726487485, 37.14960608071593384 ) ) ;
#14940 = CARTESIAN_POINT ( 'NONE',  ( 45.74753988029933538, 68.06518717409397823, 30.44471234641811819 ) ) ;
#14941 = CARTESIAN_POINT ( 'NONE',  ( 41.46631938032478359, 96.38445800887257064, 38.96596240072933170 ) ) ;
#14942 = CARTESIAN_POINT ( 'NONE',  ( -154.3824083646099439, -157.2938272943107449, 58.62277379824867296 ) ) ;
#14943 = CARTESIAN_POINT ( 'NONE',  ( 26.17254549292281496, -61.68114226949890622, 10.00000000000001599 ) ) ;
#14944 = CARTESIAN_POINT ( 'NONE',  ( -143.3790856849358306, -180.3630981290893089, 55.53486410454105027 ) ) ;
#14945 = CARTESIAN_POINT ( 'NONE',  ( -157.6495955161842062, -191.9391397928654612, 41.15050349809589392 ) ) ;
#14946 = CARTESIAN_POINT ( 'NONE',  ( 38.01140435219951996, 155.6344580088725706, 32.58608133808903773 ) ) ;
#14947 = CARTESIAN_POINT ( 'NONE',  ( 45.74753988029933538, 127.4297705074273068, 37.97664729208901946 ) ) ;
#14948 = CARTESIAN_POINT ( 'NONE',  ( 75.41016232129729246, 131.2110917358880045, 18.21592158385217886 ) ) ;
#14949 = CARTESIAN_POINT ( 'NONE',  ( 38.58424406990786082, 120.1151871740940038, 34.21067981925357060 ) ) ;
#14950 = CARTESIAN_POINT ( 'NONE',  ( -157.6495955161842062, -182.9391397928654612, 41.15050349809589392 ) ) ;
#14951 = CARTESIAN_POINT ( 'NONE',  ( 43.01140435219951996, 10.71049967264875491, 34.21067981925357060 ) ) ;
#14952 = CARTESIAN_POINT ( 'NONE',  ( 48.01140435219951996, 140.3604996726487002, 32.58608133808903773 ) ) ;
#14953 = CARTESIAN_POINT ( 'NONE',  ( 76.87285023715404009, 124.3600315475450486, -0.5611826874715375446 ) ) ;
#14954 = CARTESIAN_POINT ( 'NONE',  ( 14.94677925004173957, 122.6663546818147381, -4.724578312614759135 ) ) ;
#14955 = CARTESIAN_POINT ( 'NONE',  ( 46.59305225739526435, 97.57977050742731251, 36.81289934271958941 ) ) ;
#14956 = ORIENTED_EDGE ( 'NONE', *, *, #14390, .F. ) ;
#14957 = CIRCLE ( 'NONE', #11808, 7.500000000000007105 ) ;
#14958 = DIRECTION ( 'NONE',  ( 0.000000000000000000, 0.000000000000000000, -1.000000000000000000 ) ) ;
#14959 = EDGE_LOOP ( 'NONE', ( #8858, #11057 ) ) ;
#14960 = CARTESIAN_POINT ( 'NONE',  ( 39.92123440845004723, 86.33445800887258770, 29.95742577749337343 ) ) ;
#14961 = CARTESIAN_POINT ( 'NONE',  ( 43.01140435219951286, 59.03445800887258343, 29.21067981925356705 ) ) ;
#14962 = CARTESIAN_POINT ( 'NONE',  ( 44.55648932407425633, 136.6104996726487286, 38.96596240072933170 ) ) ;
#14964 = CARTESIAN_POINT ( 'NONE',  ( 59.61500273516548276, 97.21183980732109831, 0.7083854377657419210 ) ) ;
#14963 = CARTESIAN_POINT ( 'NONE',  ( 47.43856463449117200, 97.76518717409398107, 32.77220824515698183 ) ) ;
#14965 = EDGE_CURVE ( 'NONE', #13229, #16694, #2843, .T. ) ;
#14966 = CARTESIAN_POINT ( 'NONE',  ( -143.8425227516148084, -171.9584106276440423, 55.19815736654470584 ) ) ;
#14967 = CARTESIAN_POINT ( 'NONE',  ( -157.2955611005345986, -194.3438272943106710, 41.63779006702063867 ) ) ;
#14969 = FACE_OUTER_BOUND ( 'NONE', #12007, .T. ) ;
#14968 = DIRECTION ( 'NONE',  ( 0.000000000000000000, -1.000000000000000000, 0.000000000000000000 ) ) ;
#14970 = CARTESIAN_POINT ( 'NONE',  ( -141.4692556286852891, -188.9130981290893203, 46.40781461928724383 ) ) ;
#14971 = CARTESIAN_POINT ( 'NONE',  ( 68.01140435219951996, 119.9070776186055838, -19.99999999999997868 ) ) ;
#14972 = CARTESIAN_POINT ( 'NONE',  ( 43.01140435219951996, 151.4604996726487514, 39.21067981925356349 ) ) ;
#14973 = CARTESIAN_POINT ( 'NONE',  ( 44.82204965540741171, 59.16666133888451640, 30.14400234367970910 ) ) ;
#14974 = CARTESIAN_POINT ( 'NONE',  ( 39.92123440845005433, 62.33445800887258059, 29.95742577749336988 ) ) ;
#14975 = CARTESIAN_POINT ( 'NONE',  ( 18.20936163119166196, 143.5026679720446907, 2.934308097026923967 ) ) ;
#14976 = CARTESIAN_POINT ( 'NONE',  ( 43.01140435219951286, 144.8651871740939612, 38.86567161673127657 ) ) ;
#14977 = CIRCLE ( 'NONE', #3014, 10.00000000000000888 ) ;
#14978 = CARTESIAN_POINT ( 'NONE',  ( -151.4692556286852891, -164.6438272943107108, 39.74470866294723947 ) ) ;
#14979 = CARTESIAN_POINT ( 'NONE',  ( -160.8964159109769696, -179.0084106276440252, 52.72008163687743121 ) ) ;
#14980 = ORIENTED_EDGE ( 'NONE', *, *, #20278, .T. ) ;
#14981 = CARTESIAN_POINT ( 'NONE',  ( 44.37947211624943833, 61.01518717409400239, 38.42115945441014446 ) ) ;
#14982 = CARTESIAN_POINT ( 'NONE',  ( -148.5561028927606344, -163.2584106276440536, 58.62277379824867296 ) ) ;
#14983 = CARTESIAN_POINT ( 'NONE',  ( 70.07576047146775977, 128.1116393178318731, -2.657569147260473663 ) ) ;
#14984 = CARTESIAN_POINT ( 'NONE',  ( 40.27526882409969033, 123.5651871740939924, 37.97664729208901946 ) ) ;
#14985 = EDGE_CURVE ( 'NONE', #1249, #8316, #16392, .T. ) ;
#14986 = CARTESIAN_POINT ( 'NONE',  ( 44.01981256007524479, 154.0451711359460774, -9.132611258894215212 ) ) ;
#14987 =( BOUNDED_CURVE ( )  B_SPLINE_CURVE ( 2, ( #7227, #18898, #17230, #12387, #19011, #5876, #10857, #19224, #19121, #12165, #17665, #4016, #17553 ),
 .UNSPECIFIED., .F., .F. ) 
 B_SPLINE_CURVE_WITH_KNOTS ( ( 3, 2, 2, 2, 2, 2, 3 ),
 ( 0.8750000000000000000, 0.8764705882352941124, 0.8794117647058823373, 0.8823529411764705621, 0.8852941176470587870, 0.8882352941176470118, 0.8897058823529412352 ),
 .UNSPECIFIED. ) 
 CURVE ( )  GEOMETRIC_REPRESENTATION_ITEM ( )  RATIONAL_B_SPLINE_CURVE ( ( 0.9755282581475768211, 0.9755282581475768211, 1.000000000000000000, 0.9510565162951535312, 1.000000000000000000, 0.9510565162951535312, 1.000000000000000000, 0.9510565162951535312, 1.000000000000000000, 0.9510565162951535312, 1.000000000000000000, 0.9755282581475758219, 0.9755282581475768211 ) ) 
 REPRESENTATION_ITEM ( '' )  );
#14988 = ORIENTED_EDGE ( 'NONE', *, *, #1943, .T. ) ;
#14989 = EDGE_LOOP ( 'NONE', ( #14881, #16330, #20960, #10484, #19194 ) ) ;
#14990 = ORIENTED_EDGE ( 'NONE', *, *, #7982, .T. ) ;
#14991 = EDGE_CURVE ( 'NONE', #18069, #8286, #11329, .T. ) ;
#14992 = CARTESIAN_POINT ( 'NONE',  ( 46.10157429594899270, 109.7344580088725650, 29.95742577749337343 ) ) ;
#14993 = PRODUCT ( 'Blade Pivot Hinge Pin', 'Blade Pivot Hinge Pin', '', ( #6000 ) ) ;
#14994 = CARTESIAN_POINT ( 'NONE',  ( 41.64333658814960870, 152.7797705074273438, 30.00020018409699318 ) ) ;
#14995 = AXIS2_PLACEMENT_3D ( 'NONE', #14088, #17822, #7712 ) ;
#14996 = CARTESIAN_POINT ( 'NONE',  ( 43.01140435219951286, 71.62977050742732388, 29.55568802177586463 ) ) ;
#14998 = CARTESIAN_POINT ( 'NONE',  ( 28.62772086389876947, 95.65184626908498444, 8.013395860235284829 ) ) ;
#14997 = CARTESIAN_POINT ( 'NONE',  ( 41.64333658814960870, 128.5151871740939953, 30.00020018409699318 ) ) ;
#14999 = CONICAL_SURFACE ( 'NONE', #3404, 9.000000000000007105, 0.7853981633974457255 ) ;
#15000 = EDGE_CURVE ( 'NONE', #4862, #13398, #3954, .T. ) ;
#15001 = CARTESIAN_POINT ( 'NONE',  ( 38.01140435219952707, 84.71049967264873715, 34.21067981925357060 ) ) ;
#15002 = CARTESIAN_POINT ( 'NONE',  ( 109.8528842077358405, 344.7014318495014322, 272.0939500981630204 ) ) ;
#15003 = CARTESIAN_POINT ( 'NONE',  ( 43.01140435219951286, 143.9604996726487229, 29.21067981925356705 ) ) ;
#15004 = CARTESIAN_POINT ( 'NONE',  ( 42.21948215057683029, 139.3836182503284533, 39.21067981925354928 ) ) ;
#15005 = CARTESIAN_POINT ( 'NONE',  ( 43.01140435219951286, 87.86518717409397539, 38.86567161673127657 ) ) ;
#15006 = FACE_OUTER_BOUND ( 'NONE', #11626, .T. ) ;
#15007 = CARTESIAN_POINT ( 'NONE',  ( 38.01140435219952707, 132.5604996726487457, 32.58608133808903773 ) ) ;
#15008 = ORIENTED_EDGE ( 'NONE', *, *, #8963, .F. ) ;
#15009 = CARTESIAN_POINT ( 'NONE',  ( 47.43856463449118621, 67.87977050742730967, 34.21067981925357060 ) ) ;
#15010 = CARTESIAN_POINT ( 'NONE',  ( -154.3824083646099439, -190.5584106276440650, 58.62277379824867296 ) ) ;
#15011 = VECTOR ( 'NONE', #6838, 1000.000000000000000 ) ;
#15012 = CARTESIAN_POINT ( 'NONE',  ( 14.88286428391304561, 100.3963227437532595, 8.410691821786379307 ) ) ;
#15013 = CARTESIAN_POINT ( 'NONE',  ( -157.2955611005346270, -187.7084106276440139, 57.67623309621198047 ) ) ;
#15014 = VERTEX_POINT ( 'NONE', #21054 ) ;
#15015 = ADVANCED_FACE ( 'NONE', ( #12664 ), #5934, .T. ) ;
#15016 = CARTESIAN_POINT ( 'NONE',  ( 47.43856463449117200, 154.4651871740940123, 35.64915139335016647 ) ) ;
#15017 = PRESENTATION_LAYER_ASSIGNMENT (  '', '', ( #2689 ) ) ;
#15018 = CARTESIAN_POINT ( 'NONE',  ( 162.0641828542163125, 116.7231784796025948, -19.99999999999997868 ) ) ;
#15019 = CARTESIAN_POINT ( 'NONE',  ( 45.74753988029934249, 112.4297705074273210, 37.97664729208901235 ) ) ;
#15020 = CARTESIAN_POINT ( 'NONE',  ( 20.91437931538276374, 145.9617080342048894, -10.94665030085253044 ) ) ;
#15021 = ORIENTED_EDGE ( 'NONE', *, *, #20781, .F. ) ;
#15022 = EDGE_CURVE ( 'NONE', #4009, #20322, #4279, .T. ) ;
#15023 = CARTESIAN_POINT ( 'NONE',  ( 40.03295031927941494, 147.9482203214073479, -10.20071078494585670 ) ) ;
#15024 = EDGE_LOOP ( 'NONE', ( #4205, #18108 ) ) ;
#15025 = CARTESIAN_POINT ( 'NONE',  ( 38.58424406990784661, 114.5297705074273296, 35.64915139335016647 ) ) ;
#15026 = CARTESIAN_POINT ( 'NONE',  ( -151.4692556286852891, -126.9891397928655010, 49.65701158161630957 ) ) ;
#15027 = CARTESIAN_POINT ( 'NONE',  ( 38.58424406990784661, 84.52977050742731535, 35.64915139335016647 ) ) ;
#15028 = CARTESIAN_POINT ( 'NONE',  ( 38.58424406990784661, 156.2651871740939953, 35.64915139335016647 ) ) ;
#15029 = AXIS2_PLACEMENT_3D ( 'NONE', #6439, #16349, #11501 ) ;
#15030 = CARTESIAN_POINT ( 'NONE',  ( 27.91901995959459271, 89.26896823883201648, 8.843372880480211862 ) ) ;
#15031 = CARTESIAN_POINT ( 'NONE',  ( 41.46631938032478359, 107.1844580088725820, 29.45539723777780239 ) ) ;
#15032 = PLANE ( 'NONE',  #91 ) ;
#15033 = DIRECTION ( 'NONE',  ( 0.000000000000000000, 0.000000000000000000, 1.000000000000000000 ) ) ;
#15034 = CARTESIAN_POINT ( 'NONE',  ( -157.6495955161842062, -176.0391397928654271, 58.16351966513671812 ) ) ;
#15035 = CARTESIAN_POINT ( 'NONE',  ( 173.3794444120442222, -37.13255853780189852, 19.99999999999999645 ) ) ;
#15036 = CARTESIAN_POINT ( 'NONE',  ( -154.5594255724347761, -195.0891397928654669, 40.14644641866476604 ) ) ;
#15037 = CARTESIAN_POINT ( 'NONE',  ( 43.80332655382220253, 92.88361825032846752, 29.21067981925356705 ) ) ;
#15038 = CARTESIAN_POINT ( 'NONE',  ( 41.64333658814960870, 93.97977050742733240, 38.42115945441014446 ) ) ;
#15039 = CARTESIAN_POINT ( 'NONE',  ( 23.45520590541277883, 99.47716203340817742, 21.27102736060455257 ) ) ;
#15040 = CARTESIAN_POINT ( 'NONE',  ( -142.0420953463935803, -186.5438272943107449, 52.72008163687743831 ) ) ;
#15041 = CARTESIAN_POINT ( 'NONE',  ( 43.01140435219951286, 89.36518717409398960, 29.55568802177586107 ) ) ;
#15042 = VECTOR ( 'NONE', #8193, 1000.000000000000000 ) ;
#15043 = PLANE ( 'NONE',  #10151 ) ;
#15044 = ORIENTED_EDGE ( 'NONE', *, *, #21327, .T. ) ;
#15045 = EDGE_CURVE ( 'NONE', #6394, #13462, #5845, .T. ) ;
#15046 = CARTESIAN_POINT ( 'NONE',  ( 43.01140435219951286, 137.0344580088725763, 29.21067981925356705 ) ) ;
#15047 = FACE_OUTER_BOUND ( 'NONE', #12250, .T. ) ;
#15048 = CARTESIAN_POINT ( 'NONE',  ( 43.01140435219951286, 140.6297705074273097, 29.55568802177586107 ) ) ;
#15049 = CARTESIAN_POINT ( 'NONE',  ( 16.96697132366095673, 109.3049078165896901, 2.732358569689224748 ) ) ;
#15050 = LINE ( 'NONE', #15162, #6202 ) ;
#15051 = EDGE_LOOP ( 'NONE', ( #20539, #17718 ) ) ;
#15052 = CARTESIAN_POINT ( 'NONE',  ( 39.42975644700377558, 141.0797705074273267, 31.60846029578754468 ) ) ;
#15053 = APPLICATION_CONTEXT ( 'automotive_design' ) ;
#15054 = CARTESIAN_POINT ( 'NONE',  ( 43.01140435219951286, 95.62977050742732388, 29.55568802177586463 ) ) ;
#15055 = CARTESIAN_POINT ( 'NONE',  ( -154.5594255724347761, -192.9630981290893317, 59.16757674456785310 ) ) ;
#15056 = VECTOR ( 'NONE', #4912, 1000.000000000000000 ) ;
#15057 = CARTESIAN_POINT ( 'NONE',  ( 47.05648932407426344, 113.5104996726487485, 31.27175355779120025 ) ) ;
#15058 = CARTESIAN_POINT ( 'NONE',  ( 44.37947211624943833, 59.21518717409400523, 30.00020018409699318 ) ) ;
#15059 = LINE ( 'NONE', #13835, #12385 ) ;
#15060 = CARTESIAN_POINT ( 'NONE',  ( -160.8964159109769696, -163.7438272943107336, 52.72008163687743121 ) ) ;
#15061 = CARTESIAN_POINT ( 'NONE',  ( 41.46631938032478359, 155.1844580088725820, 29.45539723777780239 ) ) ;
#15062 = CARTESIAN_POINT ( 'NONE',  ( -141.4692556286852891, -168.0630981290893260, 49.65701158161630957 ) ) ;
#15063 =( GEOMETRIC_REPRESENTATION_CONTEXT ( 3 ) GLOBAL_UNCERTAINTY_ASSIGNED_CONTEXT ( ( #2240 ) ) GLOBAL_UNIT_ASSIGNED_CONTEXT ( ( #9375, #14322, #17841 ) ) REPRESENTATION_CONTEXT ( 'NONE', 'WORKASPACE' ) );
#15064 = CARTESIAN_POINT ( 'NONE',  ( 38.01140435219951996, 149.9344580088725820, 35.83527830041810347 ) ) ;
#15065 = CARTESIAN_POINT ( 'NONE',  ( 43.01140435219951286, 121.1297705074273097, 38.86567161673127657 ) ) ;
#15066 = CARTESIAN_POINT ( 'NONE',  ( 30.01547214559559507, 151.6658481390280144, 9.406004577920295873 ) ) ;
#15067 = CARTESIAN_POINT ( 'NONE',  ( 42.21948215057684450, 115.3836182503284533, 39.21067981925355639 ) ) ;
#15068 = CARTESIAN_POINT ( 'NONE',  ( 46.59305225739526435, 112.3151871740940067, 36.81289934271958941 ) ) ;
#15069 = EDGE_CURVE ( 'NONE', #1800, #6394, #9261, .T. ) ;
#15070 = DIRECTION ( 'NONE',  ( 0.000000000000000000, 1.000000000000000000, 0.000000000000000000 ) ) ;
#15071 = LINE ( 'NONE', #13422, #1695 ) ;
#15072 = CARTESIAN_POINT ( 'NONE',  ( 76.37589548207274959, 127.2077353526990748, 6.343625931721379452 ) ) ;
#15073 = CARTESIAN_POINT ( 'NONE',  ( 37.67147452025017174, 147.5968219552084122, -3.296006884014541782 ) ) ;
#15074 = LINE ( 'NONE', #4942, #18125 ) ;
#15075 = CARTESIAN_POINT ( 'NONE',  ( 47.43856463449118621, 94.87977050742732388, 34.21067981925357060 ) ) ;
#15076 = EDGE_CURVE ( 'NONE', #8286, #13722, #2954, .T. ) ;
#15077 = ORIENTED_EDGE ( 'NONE', *, *, #16609, .T. ) ;
#15078 = DIRECTION ( 'NONE',  ( 0.000000000000000000, 1.000000000000000000, 0.000000000000000000 ) ) ;
#15079 = ORIENTED_EDGE ( 'NONE', *, *, #14042, .T. ) ;
#15080 = CARTESIAN_POINT ( 'NONE',  ( 38.01140435219951996, 74.63445800887258486, 32.58608133808903773 ) ) ;
#15081 = DIRECTION ( 'NONE',  ( 1.723963091245776585E-16, 6.336983651701954299E-17, 1.000000000000000000 ) ) ;
#15082 = CARTESIAN_POINT ( 'NONE',  ( 47.05648932407426344, 140.5104996726487627, 31.27175355779120025 ) ) ;
#15084 = CARTESIAN_POINT ( 'NONE',  ( 59.05508021657500706, 143.0007772151335814, 5.589501426708507026 ) ) ;
#15083 = CARTESIAN_POINT ( 'NONE',  ( 39.42975644700377558, 101.8151871740940067, 31.60846029578754468 ) ) ;
#15085 = CARTESIAN_POINT ( 'NONE',  ( -151.4692556286852891, -166.4084106276440878, 59.56931450028537967 ) ) ;
#15086 = CARTESIAN_POINT ( 'NONE',  ( -148.5561028927606344, -188.7938272943107449, 40.69124936498395328 ) ) ;
#15088 = DIRECTION ( 'NONE',  ( 0.3450121214752275289, -0.9385982292947088190, 0.000000000000000000 ) ) ;
#15087 = DIRECTION ( 'NONE',  ( 0.000000000000000000, -1.000000000000000000, 0.000000000000000000 ) ) ;
#15089 = CARTESIAN_POINT ( 'NONE',  ( 38.01140435219952707, 105.5604996726487173, 32.58608133808903773 ) ) ;
#15090 = CARTESIAN_POINT ( 'NONE',  ( -149.8854112254399240, -176.3899795514095672, 39.65701158161629536 ) ) ;
#15091 = CARTESIAN_POINT ( 'NONE',  ( 48.01140435219951996, 80.36049967264874283, 32.58608133808903773 ) ) ;
#15092 = CARTESIAN_POINT ( 'NONE',  ( 43.01140435219951286, 154.1297705074273097, 38.86567161673127657 ) ) ;
#15093 = CARTESIAN_POINT ( 'NONE',  ( 41.46631938032478359, 62.18445800887258201, 29.45539723777780239 ) ) ;
#15094 = CARTESIAN_POINT ( 'NONE',  ( 22.46358530849972723, 92.52609567587644790, 8.053519324161520387 ) ) ;
#15095 = CARTESIAN_POINT ( 'NONE',  ( 47.43856463449117911, 148.4651871740940123, 35.64915139335015937 ) ) ;
#15096 = CARTESIAN_POINT ( 'NONE',  ( -160.8964159109769696, -161.0438272943107449, 46.59394152635518793 ) ) ;
#15097 = CARTESIAN_POINT ( 'NONE',  ( -142.0420953463935803, -177.5084106276440536, 46.59394152635518083 ) ) ;
#15098 = VERTEX_POINT ( 'NONE', #21267 ) ;
#15099 = DIRECTION ( 'NONE',  ( -0.4938165983075539223, 0.8695660798558991766, 0.000000000000000000 ) ) ;
#15100 = CARTESIAN_POINT ( 'NONE',  ( -157.2955611005346270, -160.7084106276440423, 57.67623309621198047 ) ) ;
#15101 = CARTESIAN_POINT ( 'NONE',  ( 70.90273821555796019, 124.5833669296562931, 4.485287862780372947 ) ) ;
#15102 = DIRECTION ( 'NONE',  ( -1.000000000000000000, 0.000000000000000000, 0.000000000000000000 ) ) ;
#15103 = CARTESIAN_POINT ( 'NONE',  ( 41.64333658814960870, 122.5151871740940095, 30.00020018409699318 ) ) ;
#15104 = EDGE_CURVE ( 'NONE', #3065, #7175, #12612, .T. ) ;
#15105 = EDGE_LOOP ( 'NONE', ( #3906, #17475 ) ) ;
#15106 = VERTEX_POINT ( 'NONE', #7608 ) ;
#15107 = CARTESIAN_POINT ( 'NONE',  ( -141.4692556286852891, -193.1391397928654783, 52.90620854394536821 ) ) ;
#15108 = ORIENTED_EDGE ( 'NONE', *, *, #19413, .T. ) ;
#15109 = VECTOR ( 'NONE', #19955, 1000.000000000000114 ) ;
#15110 = CARTESIAN_POINT ( 'NONE',  ( 44.37947211624943833, 158.4797705074273040, 30.00020018409699318 ) ) ;
#15111 = CIRCLE ( 'NONE', #8072, 7.500000000000000000 ) ;
#15112 = CARTESIAN_POINT ( 'NONE',  ( 44.37947211624943833, 65.47977050742731819, 30.00020018409699318 ) ) ;
#15114 = CARTESIAN_POINT ( 'NONE',  ( 58.43892221570314405, 143.5117748958429047, 4.561220828673259398 ) ) ;
#15113 = CARTESIAN_POINT ( 'NONE',  ( 38.58424406990784661, 122.9651871740939981, 32.77220824515698183 ) ) ;
#15115 = CARTESIAN_POINT ( 'NONE',  ( 43.01140435219951286, 85.46049967264870872, 39.46799094044489209 ) ) ;
#15116 = FACE_OUTER_BOUND ( 'NONE', #14136, .T. ) ;
#15117 = DIRECTION ( 'NONE',  ( -1.000000000000000000, -0.000000000000000000, -0.000000000000000000 ) ) ;
#15118 = DIRECTION ( 'NONE',  ( 0.000000000000000000, 0.000000000000000000, 1.000000000000000000 ) ) ;
#15119 = CARTESIAN_POINT ( 'NONE',  ( 38.58424406990786082, 81.11518717409398960, 34.21067981925357060 ) ) ;
#15120 = LINE ( 'NONE', #3659, #19618 ) ;
#15121 = CARTESIAN_POINT ( 'NONE',  ( -176.9699209214867892, -37.13255853780189852, 30.00000000000000000 ) ) ;
#15122 = ORIENTED_EDGE ( 'NONE', *, *, #2069, .F. ) ;
#15123 = CARTESIAN_POINT ( 'NONE',  ( 46.59305225739526435, 67.57977050742732672, 36.81289934271958941 ) ) ;
#15124 =( BOUNDED_CURVE ( )  B_SPLINE_CURVE ( 2, ( #19893, #21329, #11502, #6102, #11282, #11177, #2802, #16242, #1150, #7885, #14700, #14586, #18002 ),
 .UNSPECIFIED., .F., .T. ) 
 B_SPLINE_CURVE_WITH_KNOTS ( ( 3, 2, 2, 2, 2, 2, 3 ),
 ( 0.5514705882352941568, 0.5529411764705882693, 0.5558823529411764941, 0.5588235294117647189, 0.5617647058823529438, 0.5647058823529411686, 0.5661764705882352811 ),
 .UNSPECIFIED. ) 
 CURVE ( )  GEOMETRIC_REPRESENTATION_ITEM ( )  RATIONAL_B_SPLINE_CURVE ( ( 0.9755282581475768211, 0.9755282581475768211, 1.000000000000000000, 0.9510565162951535312, 1.000000000000000000, 0.9510565162951535312, 1.000000000000000000, 0.9510565162951535312, 1.000000000000000000, 0.9510565162951535312, 1.000000000000000000, 0.9755282581475768211, 0.9755282581475768211 ) ) 
 REPRESENTATION_ITEM ( '' )  );
#15125 = CARTESIAN_POINT ( 'NONE',  ( -143.8425227516148084, -183.9584106276440707, 55.19815736654470584 ) ) ;
#15126 = EDGE_CURVE ( 'NONE', #8531, #15585, #14310, .T. ) ;
#15127 = CARTESIAN_POINT ( 'NONE',  ( 77.21761637129371536, 122.6259224659223861, -2.498659462202352799 ) ) ;
#15128 = CARTESIAN_POINT ( 'NONE',  ( -160.8964159109769696, -179.1584106276440309, 49.65701158161630957 ) ) ;
#15129 = ORIENTED_EDGE ( 'NONE', *, *, #15195, .F. ) ;
#15130 = CARTESIAN_POINT ( 'NONE',  ( 45.74753988029933538, 151.1651871740939725, 37.97664729208901946 ) ) ;
#15131 = PRESENTATION_LAYER_ASSIGNMENT (  '', '', ( #10561 ) ) ;
#15132 = CARTESIAN_POINT ( 'NONE',  ( -148.3790856849358306, -159.3891397928654783, 40.14644641866477315 ) ) ;
#15133 = CARTESIAN_POINT ( 'NONE',  ( 41.64333658814960870, 110.7797705074273154, 30.00020018409699318 ) ) ;
#15134 = CARTESIAN_POINT ( 'NONE',  ( 43.10205244623161036, 154.1398065127551149, -10.16071067355346358 ) ) ;
#15135 = VERTEX_POINT ( 'NONE', #5020 ) ;
#15136 = CARTESIAN_POINT ( 'NONE',  ( 37.67147452025017174, 147.5968219552084122, -3.296006884014541782 ) ) ;
#15137 = VERTEX_POINT ( 'NONE', #5436 ) ;
#15138 = CARTESIAN_POINT ( 'NONE',  ( 39.42975644700377558, 120.0797705074273267, 31.60846029578754468 ) ) ;
#15139 = CARTESIAN_POINT ( 'NONE',  ( 161.4773229304660731, 84.89323405393692212, 4.000000000000021316 ) ) ;
#15140 = CARTESIAN_POINT ( 'NONE',  ( 40.27526882409969033, 150.5651871740940067, 37.97664729208901946 ) ) ;
#15141 = CARTESIAN_POINT ( 'NONE',  ( 39.42188022582085694, 153.9507182763122159, -10.27990332573616961 ) ) ;
#15142 = STYLED_ITEM ( 'NONE', ( #13664 ), #283 ) ;
#15143 = PRESENTATION_STYLE_ASSIGNMENT (( #3248 ) ) ;
#15144 = CARTESIAN_POINT ( 'NONE',  ( 53.01140435219953417, 119.9070776186055838, -35.00000000000000000 ) ) ;
#15145 = CARTESIAN_POINT ( 'NONE',  ( -151.4692556286852891, -177.2391397928654726, 39.14238933923362396 ) ) ;
#15146 = CARTESIAN_POINT ( 'NONE',  ( -151.4692556286852891, -136.9891397928655010, 49.65701158161630957 ) ) ;
#15147 = CARTESIAN_POINT ( 'NONE',  ( 43.01140435219951996, 10.71049967264875491, 39.21067981925356349 ) ) ;
#15148 = CARTESIAN_POINT ( 'NONE',  ( 47.05648932407426344, 92.51049967264873430, 31.27175355779120025 ) ) ;
#15149 = APPLICATION_PROTOCOL_DEFINITION ( 'draft international standard', 'automotive_design', 1998, #13918 ) ;
#15150 = CARTESIAN_POINT ( 'NONE',  ( 39.92123440845005433, 99.23445800887257917, 38.46393386101375711 ) ) ;
#15151 = CARTESIAN_POINT ( 'NONE',  ( 38.58424406990784661, 90.52977050742731535, 35.64915139335016647 ) ) ;
#15152 = CARTESIAN_POINT ( 'NONE',  ( 70.35668680342836012, 113.0167181193761508, -8.057780719902234878 ) ) ;
#15153 = CARTESIAN_POINT ( 'NONE',  ( -151.4692556286852891, -178.1438272943106824, 59.56931450028537967 ) ) ;
#15154 = EDGE_CURVE ( 'NONE', #7040, #21732, #16905, .T. ) ;
#15155 = CARTESIAN_POINT ( 'NONE',  ( 47.43856463449117911, 91.46518717409399812, 35.64915139335015937 ) ) ;
#15156 = CYLINDRICAL_SURFACE ( 'NONE', #7261, 4.999999999999997335 ) ;
#15157 = ORIENTED_EDGE ( 'NONE', *, *, #21322, .T. ) ;
#15158 = DIRECTION ( 'NONE',  ( 0.000000000000000000, 1.000000000000000000, 0.000000000000000000 ) ) ;
#15159 = CARTESIAN_POINT ( 'NONE',  ( 8.798315742295939046, 121.0924013121165075, 9.124689178586496752 ) ) ;
#15160 = CARTESIAN_POINT ( 'NONE',  ( 47.43856463449117911, 142.7297705074273324, 35.64915139335015937 ) ) ;
#15161 = CARTESIAN_POINT ( 'NONE',  ( 15.65696388169908104, 126.4253507882334588, -3.577328847893908925 ) ) ;
#15162 = CARTESIAN_POINT ( 'NONE',  ( 129.2454342010813662, 193.1635054290503319, -44.99999999999997158 ) ) ;
#15163 = EDGE_CURVE ( 'NONE', #16393, #1305, #17222, .T. ) ;
#15164 = ORIENTED_EDGE ( 'NONE', *, *, #5643, .F. ) ;
#15165 = CARTESIAN_POINT ( 'NONE',  ( 41.64333658814960870, 141.9797705074273324, 38.42115945441014446 ) ) ;
#15166 = CARTESIAN_POINT ( 'NONE',  ( 44.37947211624943833, 94.27977050742731535, 38.42115945441014446 ) ) ;
#15167 = CARTESIAN_POINT ( 'NONE',  ( 151.4773229304660731, 84.89323405393692212, 4.000000000000021316 ) ) ;
#15168 = EDGE_CURVE ( 'NONE', #8458, #19770, #5336, .T. ) ;
#15169 = EDGE_CURVE ( 'NONE', #5516, #13269, #18462, .T. ) ;
#15170 = CARTESIAN_POINT ( 'NONE',  ( 44.82204145925543060, 59.16666223754087639, 30.14399968058849666 ) ) ;
#15171 = CARTESIAN_POINT ( 'NONE',  ( -159.5594255724347761, -169.8630981290893089, 43.77915905869157598 ) ) ;
#15172 = B_SPLINE_CURVE_WITH_KNOTS ( 'NONE', 3,
 ( #2216, #17088, #18972, #13679, #2002, #20522, #2318, #12347, #14001, #8733, #13891, #20735, #15552, #20413, #3875, #12127, #351, #235, #18860, #15451, #7301, #556, #3984, #15766, #7186, #11920, #3767, #20629, #7081, #13783, #10709, #7406, #5309, #17412, #10494, #5511 ),
 .UNSPECIFIED., .F., .F.,
 ( 4, 2, 2, 2, 2, 2, 2, 2, 2, 2, 2, 2, 2, 2, 2, 2, 2, 4 ),
 ( 6.938893903907227607E-18, 0.0009794911224654321950, 0.001958982244930857451, 0.002938473367396282274, 0.003917964489861707963, 0.004897455612327133653, 0.005876946734792557608, 0.006856437857257983298, 0.007835928979723408988, 0.008815420102188832943, 0.009794911224654260368, 0.01028465678588698189, 0.01077440234711970514, 0.01175389346958513430, 0.01273338459205056693, 0.01371287571451599609, 0.01469236683698142872, 0.01567185795944685614 ),
 .UNSPECIFIED. ) ;
#15173 = CARTESIAN_POINT ( 'NONE',  ( -145.6429501568359797, -162.8438272943106995, 57.67623309621197336 ) ) ;
#15174 = DIRECTION ( 'NONE',  ( -0.9393725726208707050, -0.3428981916074316239, -0.000000000000000000 ) ) ;
#15175 = CARTESIAN_POINT ( 'NONE',  ( -143.3790856849358306, -168.3630981290893089, 55.53486410454105027 ) ) ;
#15176 =( LENGTH_UNIT ( ) NAMED_UNIT ( * ) SI_UNIT ( .MILLI., .METRE. ) );
#15177 = CARTESIAN_POINT ( 'NONE',  ( 38.96631938032478359, 146.4844580088725934, 31.27175355779120025 ) ) ;
#15178 = CARTESIAN_POINT ( 'NONE',  ( 47.43856463449117200, 122.0297705074273011, 32.77220824515698183 ) ) ;
#15179 = CARTESIAN_POINT ( 'NONE',  ( 10.92950091243491251, 131.9893946842779542, 22.49106082041198107 ) ) ;
#15180 = CARTESIAN_POINT ( 'NONE',  ( 44.55648932407425633, 99.68445800887256780, 38.96596240072933170 ) ) ;
#15181 = CARTESIAN_POINT ( 'NONE',  ( 47.43856463449117911, 121.4651871740939981, 35.64915139335015937 ) ) ;
#15182 = CARTESIAN_POINT ( 'NONE',  ( -151.4692556286852607, -168.2391397928654442, 39.65701158161629536 ) ) ;
#15183 = CYLINDRICAL_SURFACE ( 'NONE', #15760, 10.00000000000000888 ) ;
#15184 = B_SPLINE_CURVE_WITH_KNOTS ( 'NONE', 1,
 ( #16972, #3440 ),
 .UNSPECIFIED., .F., .F.,
 ( 2, 2 ),
 ( 0.000000000000000000, 1.000000000000000000 ),
 .UNSPECIFIED. ) ;
#15185 = CARTESIAN_POINT ( 'NONE',  ( 8.933461960486459574, 117.6319094064757422, 3.010161695468211551 ) ) ;
#15186 = CARTESIAN_POINT ( 'NONE',  ( 18.92353847440636727, 134.5693106245527702, 2.775393258647981920 ) ) ;
#15187 = PRODUCT ( 'bolt', 'bolt', '', ( #18008 ) ) ;
#15188 = DIRECTION ( 'NONE',  ( -1.000000000000000000, 0.000000000000000000, 0.000000000000000000 ) ) ;
#15189 = CARTESIAN_POINT ( 'NONE',  ( 45.74753988029934249, 82.42977050742732104, 37.97664729208901235 ) ) ;
#15190 =( BOUNDED_CURVE ( )  B_SPLINE_CURVE ( 2, ( #19003, #7657, #910, #19113, #14241, #5977, #17545, #587, #19321, #14134, #2347, #2242, #20872 ),
 .UNSPECIFIED., .F., .F. ) 
 B_SPLINE_CURVE_WITH_KNOTS ( ( 3, 2, 2, 2, 2, 2, 3 ),
 ( 0.5073529411764705621, 0.5088235294117646745, 0.5117647058823528994, 0.5147058823529411242, 0.5176470588235294601, 0.5205882352941176849, 0.5220588235294117974 ),
 .UNSPECIFIED. ) 
 CURVE ( )  GEOMETRIC_REPRESENTATION_ITEM ( )  RATIONAL_B_SPLINE_CURVE ( ( 0.9755282581475768211, 0.9755282581475768211, 1.000000000000000000, 0.9510565162951535312, 1.000000000000000000, 0.9510565162951535312, 1.000000000000000000, 0.9510565162951535312, 1.000000000000000000, 0.9510565162951535312, 1.000000000000000000, 0.9755282581475768211, 0.9755282581475768211 ) ) 
 REPRESENTATION_ITEM ( '' )  );
#15191 = ORIENTED_EDGE ( 'NONE', *, *, #13509, .T. ) ;
#15192 = FACE_BOUND ( 'NONE', #2932, .T. ) ;
#15193 = CARTESIAN_POINT ( 'NONE',  ( 38.01140435219952707, 74.78445800887257633, 34.21067981925357060 ) ) ;
#15194 = DIRECTION ( 'NONE',  ( 0.000000000000000000, 1.000000000000000000, 0.000000000000000000 ) ) ;
#15195 = EDGE_CURVE ( 'NONE', #13122, #3596, #14852, .T. ) ;
#15196 = CARTESIAN_POINT ( 'NONE',  ( 47.05648932407426344, 131.5104996726487343, 31.27175355779120025 ) ) ;
#15198 = CARTESIAN_POINT ( 'NONE',  ( 50.52618006956270591, 153.2232370340747138, -15.91843667049845834 ) ) ;
#15197 = CARTESIAN_POINT ( 'NONE',  ( 39.42975644700377558, 83.81518717409400665, 31.60846029578754468 ) ) ;
#15199 = CARTESIAN_POINT ( 'NONE',  ( -156.1828684652448658, -155.6591478762521490, 41.49287016839723918 ) ) ;
#15200 = CARTESIAN_POINT ( 'NONE',  ( -143.8425227516148084, -195.0938272943107279, 44.11586579668791330 ) ) ;
#15201 = CARTESIAN_POINT ( 'NONE',  ( 43.01140435219951996, 10.71049967264875491, 34.21067981925357060 ) ) ;
#15202 = CARTESIAN_POINT ( 'NONE',  ( 46.10157429594899270, 126.8344580088725593, 38.46393386101375711 ) ) ;
#15203 = CIRCLE ( 'NONE', #16239, 10.00000000000000888 ) ;
#15204 = VECTOR ( 'NONE', #10906, 1000.000000000000114 ) ;
#15205 = DIRECTION ( 'NONE',  ( 0.000000000000000000, 1.000000000000000000, 0.000000000000000000 ) ) ;
#15206 = DIRECTION ( 'NONE',  ( 0.000000000000000000, -0.000000000000000000, 1.000000000000000000 ) ) ;
#15207 = CARTESIAN_POINT ( 'NONE',  ( 43.01140435219951286, 152.6297705074272812, 29.55568802177586463 ) ) ;
#15208 = CARTESIAN_POINT ( 'NONE',  ( 43.01140435219951286, 63.53445800887256922, 39.21067981925356349 ) ) ;
#15209 = CARTESIAN_POINT ( 'NONE',  ( 13.33420504782278293, 102.8437529505761603, 1.505736668420971869 ) ) ;
#15210 = CARTESIAN_POINT ( 'NONE',  ( 38.58424406990785371, 147.2651871740939669, 35.64915139335015937 ) ) ;
#15211 = AXIS2_PLACEMENT_3D ( 'NONE', #17243, #4134, #17459 ) ;
#15212 = CARTESIAN_POINT ( 'NONE',  ( -151.4692556286852891, -166.1438272943107393, 59.56931450028537967 ) ) ;
#15213 = CARTESIAN_POINT ( 'NONE',  ( -145.6429501568359797, -174.2084106276440139, 41.63779006702063867 ) ) ;
#15214 = ORIENTED_EDGE ( 'NONE', *, *, #15104, .T. ) ;
#15215 = CARTESIAN_POINT ( 'NONE',  ( 47.43856463449117911, 61.46518717409398391, 35.64915139335015937 ) ) ;
#15216 = CARTESIAN_POINT ( 'NONE',  ( -143.8425227516148084, -162.3584106276440480, 44.11586579668791330 ) ) ;
#15217 = CARTESIAN_POINT ( 'NONE',  ( 23.20524185134216921, 147.9029287973646660, 23.16022673208204807 ) ) ;
#15218 = CARTESIAN_POINT ( 'NONE',  ( 39.42975644700377558, 126.4151871740940010, 36.81289934271958941 ) ) ;
#15219 = VERTEX_POINT ( 'NONE', #51 ) ;
#15220 = VERTEX_POINT ( 'NONE', #10202 ) ;
#15221 = AXIS2_PLACEMENT_3D ( 'NONE', #7928, #7823, #16179 ) ;
#15222 = AXIS2_PLACEMENT_3D ( 'NONE', #14522, #6368, #9474 ) ;
#15223 = CARTESIAN_POINT ( 'NONE',  ( 38.96631938032478359, 147.0844580088725877, 37.14960608071593384 ) ) ;
#15224 = EDGE_LOOP ( 'NONE', ( #2569, #16701, #6671, #13158 ) ) ;
#15225 = CARTESIAN_POINT ( 'NONE',  ( 46.10157429594899270, 99.83445800887257349, 38.46393386101376421 ) ) ;
#15226 = CARTESIAN_POINT ( 'NONE',  ( 41.64333658814960870, 155.7797705074273438, 30.00020018409699318 ) ) ;
#15227 = AXIS2_PLACEMENT_3D ( 'NONE', #1812, #15370, #6787 ) ;
#15228 = CARTESIAN_POINT ( 'NONE',  ( 41.64333658814960870, 65.77977050742732956, 30.00020018409699318 ) ) ;
#15230 = CARTESIAN_POINT ( 'NONE',  ( 40.25662930883660806, 147.8909896968035014, -16.19631701608006580 ) ) ;
#15229 = CARTESIAN_POINT ( 'NONE',  ( 43.01140435219951286, 120.8651871740940180, 38.86567161673127657 ) ) ;
#15231 = CARTESIAN_POINT ( 'NONE',  ( 46.10157429594899270, 83.66049967264873999, 29.95742577749337343 ) ) ;
#15232 = CARTESIAN_POINT ( 'NONE',  ( -151.4692556286852891, -196.9891397928655010, 49.65701158161630957 ) ) ;
#15233 = CARTESIAN_POINT ( 'NONE',  ( -143.3790856849358306, -171.3630981290893089, 55.53486410454105027 ) ) ;
#15234 = DIRECTION ( 'NONE',  ( 1.000000000000000000, 0.000000000000000000, 0.000000000000000000 ) ) ;
#15235 = CARTESIAN_POINT ( 'NONE',  ( 45.74753988029933538, 76.16518717409400097, 37.97664729208901946 ) ) ;
#15236 = PRODUCT_DEFINITION_CONTEXT ( 'detailed design', #8307, 'design' ) ;
#15237 = CARTESIAN_POINT ( 'NONE',  ( 43.01140435219951996, 144.9070776186055696, 29.21067981925357060 ) ) ;
#15238 = DIRECTION ( 'NONE',  ( -1.000000000000000000, 0.000000000000000000, 0.000000000000000000 ) ) ;
#15239 = ORIENTED_EDGE ( 'NONE', *, *, #21656, .F. ) ;
#15240 = CARTESIAN_POINT ( 'NONE',  ( 38.58424406990784661, 69.52977050742730114, 35.64915139335016647 ) ) ;
#15241 = CARTESIAN_POINT ( 'NONE',  ( -142.0420953463935803, -183.5084106276440252, 46.59394152635518793 ) ) ;
#15242 = CARTESIAN_POINT ( 'NONE',  ( 51.83766784316492249, 86.74794057323931895, -0.9509610611041249273 ) ) ;
#15243 = CARTESIAN_POINT ( 'NONE',  ( -142.0420953463935803, -177.8084106276440650, 52.72008163687743831 ) ) ;
#15244 = ORIENTED_EDGE ( 'NONE', *, *, #17566, .F. ) ;
#15245 = CARTESIAN_POINT ( 'NONE',  ( 47.43856463449118621, 157.6151871740940180, 34.21067981925357060 ) ) ;
#15246 = LINE ( 'NONE', #18662, #13092 ) ;
#15247 = CARTESIAN_POINT ( 'NONE',  ( 45.74753988029934249, 118.4297705074272926, 37.97664729208901235 ) ) ;
#15248 = CARTESIAN_POINT ( 'NONE',  ( 77.19215121279506775, 118.0176990621192203, -1.351406188750652992 ) ) ;
#15249 = VERTEX_POINT ( 'NONE', #10309 ) ;
#15250 = CARTESIAN_POINT ( 'NONE',  ( 51.94691807752363388, 146.6530262932614050, -9.724486432582017059 ) ) ;
#15251 = VERTEX_POINT ( 'NONE', #17012 ) ;
#15252 = CARTESIAN_POINT ( 'NONE',  ( 173.3794444120442506, -84.13255853780189852, 20.00000000000001776 ) ) ;
#15253 = CARTESIAN_POINT ( 'NONE',  ( 46.59305225739526435, 86.17977050742732104, 31.60846029578754468 ) ) ;
#15254 = CARTESIAN_POINT ( 'NONE',  ( 38.58424406990784661, 152.9651871740940123, 32.77220824515698183 ) ) ;
#15255 = CARTESIAN_POINT ( 'NONE',  ( 31.29766364123476663, 87.82482650329993135, 8.724447585906515812 ) ) ;
#15256 = CARTESIAN_POINT ( 'NONE',  ( -59.65946286876558702, 788.4655180356369328, -6.999999999999995559 ) ) ;
#15257 = CYLINDRICAL_SURFACE ( 'NONE', #3246, 4.999999999999997335 ) ;
#15258 = ADVANCED_FACE ( 'NONE', ( #1919 ), #9300, .T. ) ;
#15259 = CARTESIAN_POINT ( 'NONE',  ( -151.4692556286852891, -183.2391397928654726, 39.14238933923362396 ) ) ;
#15260 = DIRECTION ( 'NONE',  ( 0.000000000000000000, 0.000000000000000000, 1.000000000000000000 ) ) ;
#15261 = UNCERTAINTY_MEASURE_WITH_UNIT (LENGTH_MEASURE( 1.000000000000000082E-05 ), #12975, 'distance_accuracy_value', 'NONE');
#15262 = CARTESIAN_POINT ( 'NONE',  ( -151.4692556286853176, -173.3130981290892976, 39.65701158161629536 ) ) ;
#15263 = CARTESIAN_POINT ( 'NONE',  ( 47.05648932407426344, 97.58445800887258770, 31.27175355779120025 ) ) ;
#15264 = CARTESIAN_POINT ( 'NONE',  ( 42.21948215057684450, 99.45757658655229250, 39.21067981925355639 ) ) ;
#15265 = CARTESIAN_POINT ( 'NONE',  ( 44.37947211624943833, 98.47977050742731819, 30.00020018409699318 ) ) ;
#15266 = CARTESIAN_POINT ( 'NONE',  ( 66.79315400704923888, 104.7533658121278819, -7.700889860664787534 ) ) ;
#15267 = CARTESIAN_POINT ( 'NONE',  ( -148.5561028927606344, -174.9938272943107336, 58.62277379824867296 ) ) ;
#15268 = CARTESIAN_POINT ( 'NONE',  ( 47.43856463449117911, 82.76518717409400949, 32.77220824515697473 ) ) ;
#15269 = LINE ( 'NONE', #2039, #15357 ) ;
#15270 = ORIENTED_EDGE ( 'NONE', *, *, #5441, .F. ) ;
#15271 = CARTESIAN_POINT ( 'NONE',  ( 38.01140435219952707, 137.6344580088725706, 32.58608133808903773 ) ) ;
#15272 = CARTESIAN_POINT ( 'NONE',  ( 11.08170843061617816, 132.1625483722078513, 16.49545033792581350 ) ) ;
#15273 = CARTESIAN_POINT ( 'NONE',  ( 19.10471955674299238, 134.7123306330852870, -3.220215631267630219 ) ) ;
#15274 = VECTOR ( 'NONE', #13470, 1000.000000000000000 ) ;
#15275 = ADVANCED_FACE ( 'NONE', ( #11047 ), #10849, .F. ) ;
#15276 = CARTESIAN_POINT ( 'NONE',  ( 47.43856463449118621, 61.87977050742732388, 34.21067981925357060 ) ) ;
#15277 = VERTEX_POINT ( 'NONE', #19427 ) ;
#15278 = CARTESIAN_POINT ( 'NONE',  ( 43.01140435219951286, 146.6297705074273381, 29.55568802177586463 ) ) ;
#15279 = EDGE_CURVE ( 'NONE', #10182, #11010, #9410, .T. ) ;
#15281 = EDGE_CURVE ( 'NONE', #4552, #15878, #805, .T. ) ;
#15280 = LINE ( 'NONE', #18477, #16497 ) ;
#15282 = CARTESIAN_POINT ( 'NONE',  ( 47.43856463449118621, 61.61518717409400381, 34.21067981925357060 ) ) ;
#15283 = CARTESIAN_POINT ( 'NONE',  ( -157.6495955161842062, -170.0130981290892862, 41.15050349809589392 ) ) ;
#15284 = VECTOR ( 'NONE', #6735, 1000.000000000000114 ) ;
#15285 = EDGE_CURVE ( 'NONE', #13720, #18280, #954, .T. ) ;
#15286 = LINE ( 'NONE', #18806, #5882 ) ;
#15287 = FACE_OUTER_BOUND ( 'NONE', #13298, .T. ) ;
#15288 = CARTESIAN_POINT ( 'NONE',  ( -145.2889157411863721, -165.5130981290892862, 58.16351966513671812 ) ) ;
#15289 = DIRECTION ( 'NONE',  ( -0.000000000000000000, -0.000000000000000000, -1.000000000000000000 ) ) ;
#15290 = CARTESIAN_POINT ( 'NONE',  ( 46.10157429594899270, 139.7344580088725934, 29.95742577749337343 ) ) ;
#15291 = CARTESIAN_POINT ( 'NONE',  ( 47.43856463449117200, 119.0297705074273296, 32.77220824515698183 ) ) ;
#15292 = CARTESIAN_POINT ( 'NONE',  ( 9.116869730174032682, 125.2576736736073428, 22.26325814793822744 ) ) ;
#15293 = PLANE ( 'NONE',  #17663 ) ;
#15294 = CARTESIAN_POINT ( 'NONE',  ( 46.59305225739526435, 106.9151871740940152, 31.60846029578754468 ) ) ;
#15295 = CARTESIAN_POINT ( 'NONE',  ( 39.92123440845005433, 125.3344580088725735, 29.95742577749336988 ) ) ;
#15296 = CARTESIAN_POINT ( 'NONE',  ( 17.06177112331949886, 97.70250936324737268, 2.295960169688653352 ) ) ;
#15297 = CARTESIAN_POINT ( 'NONE',  ( 53.00431643774457768, 93.53749527547704190, -6.986323292181506162 ) ) ;
#15298 = DIRECTION ( 'NONE',  ( -1.000000000000000000, 0.000000000000000000, 0.000000000000000000 ) ) ;
#15299 = ADVANCED_FACE ( 'NONE', ( #9195 ), #17762, .T. ) ;
#15300 = CARTESIAN_POINT ( 'NONE',  ( 46.59305225739526435, 88.57977050742732672, 36.81289934271958941 ) ) ;
#15301 = VECTOR ( 'NONE', #9465, 1000.000000000000000 ) ;
#15302 = EDGE_CURVE ( 'NONE', #14339, #7314, #20659, .T. ) ;
#15303 = CARTESIAN_POINT ( 'NONE',  ( -151.4692556286852607, -168.8130981290893260, 59.65701158161632378 ) ) ;
#15304 = AXIS2_PLACEMENT_3D ( 'NONE', #18725, #20495, #13650 ) ;
#15305 = CARTESIAN_POINT ( 'NONE',  ( 39.92123440845004723, 69.23445800887259338, 38.46393386101376421 ) ) ;
#15306 = CARTESIAN_POINT ( 'NONE',  ( 39.92123440845005433, 59.33445800887256638, 29.95742577749336988 ) ) ;
#15307 = CARTESIAN_POINT ( 'NONE',  ( 39.92123440845004723, 126.2604996726487485, 29.95742577749337343 ) ) ;
#15309 = CARTESIAN_POINT ( 'NONE',  ( 44.19315180539718568, 85.77372119115894122, -12.70412401877768005 ) ) ;
#15308 = CARTESIAN_POINT ( 'NONE',  ( 46.59305225739526435, 82.91518717409400097, 31.60846029578754468 ) ) ;
#15310 = CARTESIAN_POINT ( 'NONE',  ( -145.6429501568359797, -159.2084106276439854, 41.63779006702063867 ) ) ;
#15311 = CARTESIAN_POINT ( 'NONE',  ( -143.8425227516148084, -177.0938272943107279, 44.11586579668791330 ) ) ;
#15312 = CYLINDRICAL_SURFACE ( 'NONE', #5835, 4.999999999999997335 ) ;
#15313 = CARTESIAN_POINT ( 'NONE',  ( -151.4692556286852891, -194.3130981290892976, 39.14238933923362396 ) ) ;
#15314 = CARTESIAN_POINT ( 'NONE',  ( 38.01140435219952707, 92.93445800887258201, 35.83527830041809636 ) ) ;
#15315 = CARTESIAN_POINT ( 'NONE',  ( -39.63192160874135084, -136.9891397928655010, 20.00000000000002132 ) ) ;
#15316 = CARTESIAN_POINT ( 'NONE',  ( 38.58424406990784661, 150.5297705074272869, 35.64915139335016647 ) ) ;
#15317 = FACE_OUTER_BOUND ( 'NONE', #9103, .T. ) ;
#15318 = EDGE_CURVE ( 'NONE', #12255, #7439, #15190, .T. ) ;
#15319 = CARTESIAN_POINT ( 'NONE',  ( 20.69791174355615837, 145.8831102580302570, -4.951040100860263138 ) ) ;
#15320 = CARTESIAN_POINT ( 'NONE',  ( 45.74753988029934249, 146.0651871740940067, 30.44471234641812174 ) ) ;
#15321 = CARTESIAN_POINT ( 'NONE',  ( -157.6495955161842062, -188.0391397928654555, 58.16351966513671812 ) ) ;
#15322 = CARTESIAN_POINT ( 'NONE',  ( -160.8964159109769696, -173.1584106276440593, 49.65701158161630957 ) ) ;
#15323 = CARTESIAN_POINT ( 'NONE',  ( 47.43856463449117911, 61.76518717409399528, 32.77220824515697473 ) ) ;
#15324 =( BOUNDED_CURVE ( )  B_SPLINE_CURVE ( 2, ( #10779, #524, #17593, #17485, #19259, #14072, #2395, #7584, #20592, #19150, #10460, #14180, #9132 ),
 .UNSPECIFIED., .F., .F. ) 
 B_SPLINE_CURVE_WITH_KNOTS ( ( 3, 2, 2, 2, 2, 2, 3 ),
 ( 0.6964285714285713969, 0.6999999999999999556, 0.7071428571428571841, 0.7142857142857143016, 0.7214285714285714191, 0.7285714285714285365, 0.7321428571428572063 ),
 .UNSPECIFIED. ) 
 CURVE ( )  GEOMETRIC_REPRESENTATION_ITEM ( )  RATIONAL_B_SPLINE_CURVE ( ( 0.9755282581475768211, 0.9755282581475768211, 1.000000000000000000, 0.9510565162951535312, 1.000000000000000000, 0.9510565162951535312, 1.000000000000000000, 0.9510565162951535312, 1.000000000000000000, 0.9510565162951535312, 1.000000000000000000, 0.9755282581475763770, 0.9755282581475768211 ) ) 
 REPRESENTATION_ITEM ( '' )  );
#15325 = CARTESIAN_POINT ( 'NONE',  ( -151.4692556286852891, -161.9084106276440593, 39.74470866294723947 ) ) ;
#15326 = CARTESIAN_POINT ( 'NONE',  ( 64.22416581780682066, 138.6102112617928128, -3.133847767204844370 ) ) ;
#15327 = VECTOR ( 'NONE', #17034, 1000.000000000000114 ) ;
#15328 = DIRECTION ( 'NONE',  ( -0.000000000000000000, 1.000000000000000000, -0.000000000000000000 ) ) ;
#15329 = CARTESIAN_POINT ( 'NONE',  ( 46.59305225739526435, 121.9151871740940010, 31.60846029578754468 ) ) ;
#15330 = ORIENTED_EDGE ( 'NONE', *, *, #12070, .F. ) ;
#15331 = ORIENTED_EDGE ( 'NONE', *, *, #18525, .F. ) ;
#15332 = DIRECTION ( 'NONE',  ( 1.000000000000000000, 0.000000000000000000, 0.000000000000000000 ) ) ;
#15333 = EDGE_LOOP ( 'NONE', ( #7548, #3090, #16968, #1109 ) ) ;
#15334 = CARTESIAN_POINT ( 'NONE',  ( 44.55648932407425633, 102.6844580088725820, 38.96596240072933170 ) ) ;
#15335 = CARTESIAN_POINT ( 'NONE',  ( 43.01140435219951996, 157.4604996726487514, 39.21067981925355639 ) ) ;
#15336 = CARTESIAN_POINT ( 'NONE',  ( 38.96631938032478359, 159.4104996726487400, 31.27175355779120025 ) ) ;
#15338 = CARTESIAN_POINT ( 'NONE',  ( 68.77576173894735234, 108.4446202281264249, 13.13264940013829296 ) ) ;
#15337 = CARTESIAN_POINT ( 'NONE',  ( 40.27526882409969033, 114.5651871740939782, 37.97664729208901946 ) ) ;
#15339 = CARTESIAN_POINT ( 'NONE',  ( 48.01140435219951996, 71.36049967264874283, 32.58608133808903773 ) ) ;
#15340 = CARTESIAN_POINT ( 'NONE',  ( 46.10157429594899270, 136.7344580088725365, 29.95742577749336988 ) ) ;
#15341 = VECTOR ( 'NONE', #3873, 1000.000000000000000 ) ;
#15342 = FACE_BOUND ( 'NONE', #20311, .T. ) ;
#15343 = DIRECTION ( 'NONE',  ( -0.000000000000000000, -0.000000000000000000, -1.000000000000000000 ) ) ;
#15344 = CARTESIAN_POINT ( 'NONE',  ( 38.58424406990784661, 74.96518717409401233, 32.77220824515698183 ) ) ;
#15345 = CARTESIAN_POINT ( 'NONE',  ( 42.35272797528494237, 144.9004681788466087, 29.24343323619035573 ) ) ;
#15346 = CARTESIAN_POINT ( 'NONE',  ( -142.0420953463935803, -180.2438272943107052, 46.59394152635518793 ) ) ;
#15347 = CARTESIAN_POINT ( 'NONE',  ( 38.96631938032478359, 132.4104996726487684, 31.27175355779120025 ) ) ;
#15348 = ORIENTED_EDGE ( 'NONE', *, *, #14052, .T. ) ;
#15349 = CARTESIAN_POINT ( 'NONE',  ( -159.0959885057557983, -181.8584106276440480, 55.19815736654470584 ) ) ;
#15350 = CARTESIAN_POINT ( 'NONE',  ( 72.04953363923264931, 101.6246461802091972, -1.784078408812360017 ) ) ;
#15351 = EDGE_CURVE ( 'NONE', #5871, #15900, #4008, .T. ) ;
#15352 = CARTESIAN_POINT ( 'NONE',  ( -143.8425227516148084, -180.3584106276440480, 44.11586579668791330 ) ) ;
#15353 = VERTEX_POINT ( 'NONE', #20763 ) ;
#15354 = APPLICATION_CONTEXT ( 'automotive_design' ) ;
#15355 = CIRCLE ( 'NONE', #12528, 21.90454335994848734 ) ;
#15356 = CARTESIAN_POINT ( 'NONE',  ( 41.64333658814960870, 155.5151871740940237, 30.00020018409699318 ) ) ;
#15357 = VECTOR ( 'NONE', #5546, 1000.000000000000000 ) ;
#15358 = DIRECTION ( 'NONE',  ( 0.000000000000000000, -1.000000000000000000, 0.000000000000000000 ) ) ;
#15359 = CARTESIAN_POINT ( 'NONE',  ( 38.58424406990785371, 117.5297705074273154, 35.64915139335015937 ) ) ;
#15360 = CARTESIAN_POINT ( 'NONE',  ( 32.14050509837299785, 87.44534670509604268, 7.696117750009315195 ) ) ;
#15361 = ORIENTED_EDGE ( 'NONE', *, *, #6294, .F. ) ;
#15362 = CARTESIAN_POINT ( 'NONE',  ( 65.02675087932300357, 102.2843278501921418, -7.581721168364237151 ) ) ;
#15363 = ORIENTED_EDGE ( 'NONE', *, *, #19592, .F. ) ;
#15364 = CARTESIAN_POINT ( 'NONE',  ( 46.59305225739526435, 109.5797705074273125, 36.81289934271958941 ) ) ;
#15365 = CARTESIAN_POINT ( 'NONE',  ( 41.46631938032478359, 131.1844580088725820, 29.45539723777780239 ) ) ;
#15366 = CARTESIAN_POINT ( 'NONE',  ( 39.92123440845005433, 129.2344580088725934, 38.46393386101375711 ) ) ;
#15367 = CARTESIAN_POINT ( 'NONE',  ( 46.59305225739526435, 148.3151871740940067, 36.81289934271958941 ) ) ;
#15368 = EDGE_CURVE ( 'NONE', #846, #10835, #5655, .T. ) ;
#15369 = CARTESIAN_POINT ( 'NONE',  ( 23.17700876947760591, 147.8092992330439586, -3.851376987104358829 ) ) ;
#15370 = DIRECTION ( 'NONE',  ( 0.007125320983193088667, 0.9999746145782334450, 0.000000000000000000 ) ) ;
#15371 = LINE ( 'NONE', #264, #15561 ) ;
#15372 = CARTESIAN_POINT ( 'NONE',  ( -161.4692556286852607, -173.6391397928654214, 46.40781461928724383 ) ) ;
#15373 = CARTESIAN_POINT ( 'NONE',  ( 24.43941541943582862, 313.3049502139530205, -19.99999999999997868 ) ) ;
#15374 = DIRECTION ( 'NONE',  ( -0.000000000000000000, 1.000000000000000000, -0.000000000000000000 ) ) ;
#15375 = CARTESIAN_POINT ( 'NONE',  ( 48.01140435219951996, 92.06049967264873146, 35.83527830041809636 ) ) ;
#15376 = AXIS2_PLACEMENT_3D ( 'NONE', #13979, #538, #758 ) ;
#15377 = AXIS2_PLACEMENT_3D ( 'NONE', #1451, #11466, #19860 ) ;
#15378 = CARTESIAN_POINT ( 'NONE',  ( 45.74753988029933538, 94.42977050742732104, 37.97664729208901946 ) ) ;
#15379 = CARTESIAN_POINT ( 'NONE',  ( 60.80507725967250821, 98.03074643439879310, -7.343579217248467295 ) ) ;
#15380 = CARTESIAN_POINT ( 'NONE',  ( -143.8425227516148084, -177.0938272943107279, 44.11586579668791330 ) ) ;
#15381 = CARTESIAN_POINT ( 'NONE',  ( 40.27526882409969744, 81.56518717409399244, 37.97664729208901235 ) ) ;
#15382 = CARTESIAN_POINT ( 'NONE',  ( -157.6495955161842062, -170.0391397928654840, 58.16351966513671812 ) ) ;
#15383 = CARTESIAN_POINT ( 'NONE',  ( -157.6495955161842062, -158.9391397928654612, 41.15050349809589392 ) ) ;
#15384 = ORIENTED_EDGE ( 'NONE', *, *, #9526, .T. ) ;
#15385 = CARTESIAN_POINT ( 'NONE',  ( -143.9637021292202235, -116.9891397928655010, 36.65701158161628825 ) ) ;
#15386 = DIRECTION ( 'NONE',  ( 0.000000000000000000, 0.000000000000000000, 1.000000000000000000 ) ) ;
#15387 = CARTESIAN_POINT ( 'NONE',  ( 71.19781441516849441, 139.1947734567256703, -15.08494495145127878 ) ) ;
#15388 = ORIENTED_EDGE ( 'NONE', *, *, #19160, .T. ) ;
#15389 = EDGE_CURVE ( 'NONE', #14823, #6453, #15789, .T. ) ;
#15390 = CARTESIAN_POINT ( 'NONE',  ( 42.21948215057684450, 119.1113394311928460, 29.21067981925356705 ) ) ;
#15391 = ORIENTED_EDGE ( 'NONE', *, *, #2276, .F. ) ;
#15392 = VECTOR ( 'NONE', #7298, 1000.000000000000114 ) ;
#15393 = CARTESIAN_POINT ( 'NONE',  ( 41.64333658814960870, 135.9797705074273324, 38.42115945441014446 ) ) ;
#15394 = DIRECTION ( 'NONE',  ( 0.000000000000000000, 0.000000000000000000, 1.000000000000000000 ) ) ;
#15395 = DIRECTION ( 'NONE',  ( 0.000000000000000000, 0.000000000000000000, 1.000000000000000000 ) ) ;
#15396 = LINE ( 'NONE', #3384, #1123 ) ;
#15397 = CARTESIAN_POINT ( 'NONE',  ( -156.1828684652451784, -155.6591478762521206, 41.49287016839741682 ) ) ;
#15398 = LINE ( 'NONE', #2160, #3436 ) ;
#15399 = CARTESIAN_POINT ( 'NONE',  ( 38.96631938032478359, 108.4104996726487400, 31.27175355779120025 ) ) ;
#15400 = CARTESIAN_POINT ( 'NONE',  ( -154.5594255724347761, -168.9630981290893033, 59.16757674456785310 ) ) ;
#15401 = CARTESIAN_POINT ( 'NONE',  ( 43.01140435219951286, 138.5344580088726048, 39.46799094044489209 ) ) ;
#15402 = CARTESIAN_POINT ( 'NONE',  ( 47.43856463449117200, 121.7297705074273040, 35.64915139335016647 ) ) ;
#15403 = CARTESIAN_POINT ( 'NONE',  ( 14.73513546934961482, 119.4163655414939740, 1.151864106104608432 ) ) ;
#15404 = CARTESIAN_POINT ( 'NONE',  ( 38.01140435219952707, 140.9344580088725820, 35.83527830041809636 ) ) ;
#15405 = AXIS2_PLACEMENT_3D ( 'NONE', #7679, #5781, #6106 ) ;
#15406 = CARTESIAN_POINT ( 'NONE',  ( 41.64333658814960870, 110.5151871740940095, 30.00020018409699318 ) ) ;
#15407 = DIRECTION ( 'NONE',  ( 0.9949940778855791423, 0.09993390301907582873, 0.000000000000000000 ) ) ;
#15408 = CARTESIAN_POINT ( 'NONE',  ( 20.75180444880664510, 93.89949152720284076, -5.875022464008872625 ) ) ;
#15409 = EDGE_CURVE ( 'NONE', #7314, #3622, #9985, .T. ) ;
#15410 = CARTESIAN_POINT ( 'NONE',  ( 46.56541826512206228, 91.93282113015048651, 0.2755065429245392439 ) ) ;
#15411 = CARTESIAN_POINT ( 'NONE',  ( -120.0322075325610740, -126.9891397928655010, 30.00000000000000000 ) ) ;
#15412 = CARTESIAN_POINT ( 'NONE',  ( 38.58424406990785371, 87.22977050742731819, 32.77220824515697473 ) ) ;
#15413 = ORIENTED_EDGE ( 'NONE', *, *, #8231, .F. ) ;
#15414 = VECTOR ( 'NONE', #3904, 1000.000000000000000 ) ;
#15415 = CARTESIAN_POINT ( 'NONE',  ( 46.10157429594899270, 134.6604996726487684, 29.95742577749336988 ) ) ;
#15416 = CARTESIAN_POINT ( 'NONE',  ( 48.01140435219951996, 73.43445800887255359, 32.58608133808903773 ) ) ;
#15417 = CARTESIAN_POINT ( 'NONE',  ( 42.21948215057684450, 60.45757658655230671, 39.21067981925355639 ) ) ;
#15418 = CIRCLE ( 'NONE', #9425, 7.500000000000007105 ) ;
#15419 = CARTESIAN_POINT ( 'NONE',  ( 48.01140435219951996, 134.0604996726486888, 35.83527830041810347 ) ) ;
#15421 = CARTESIAN_POINT ( 'NONE',  ( 51.37827275082728562, 86.79484443300951568, -12.94217320967262275 ) ) ;
#15420 = CARTESIAN_POINT ( 'NONE',  ( 46.59305225739526435, 88.91518717409400097, 31.60846029578754468 ) ) ;
#15422 = CARTESIAN_POINT ( 'NONE',  ( -143.8425227516148084, -162.9584106276440423, 55.19815736654470584 ) ) ;
#15423 = CARTESIAN_POINT ( 'NONE',  ( -148.5561028927606344, -180.9938272943107336, 58.62277379824867296 ) ) ;
#15424 = CARTESIAN_POINT ( 'NONE',  ( -141.4692556286852891, -177.8391397928654385, 46.40781461928724383 ) ) ;
#15425 = CARTESIAN_POINT ( 'NONE',  ( 43.01140435219951286, 125.9604996726487514, 29.21067981925356705 ) ) ;
#15426 = CARTESIAN_POINT ( 'NONE',  ( 42.21948215057687293, 93.45757658655232092, 39.21067981925357060 ) ) ;
#15427 = CARTESIAN_POINT ( 'NONE',  ( 43.80332655382220253, 143.8836182503284817, 29.21067981925356705 ) ) ;
#15428 = CARTESIAN_POINT ( 'NONE',  ( 38.58424406990786082, 147.3797705074273097, 34.21067981925357060 ) ) ;
#15429 = CARTESIAN_POINT ( 'NONE',  ( 39.42975644700377558, 105.0797705074273125, 31.60846029578754468 ) ) ;
#15430 = CARTESIAN_POINT ( 'NONE',  ( 15.97061701817242785, 140.8453463817331794, 16.82122940411608170 ) ) ;
#15431 = CARTESIAN_POINT ( 'NONE',  ( 44.37947211624943833, 140.2151871740940123, 30.00020018409699318 ) ) ;
#15432 = CARTESIAN_POINT ( 'NONE',  ( -161.4692556286852891, -188.3391397928654953, 52.90620854394536821 ) ) ;
#15433 = CARTESIAN_POINT ( 'NONE',  ( -160.8964159109769696, -173.0084106276440536, 52.72008163687743121 ) ) ;
#15434 = CARTESIAN_POINT ( 'NONE',  ( 15.47577296012077142, 113.4559151263126040, 0.9141320964044082897 ) ) ;
#15435 = SURFACE_STYLE_USAGE ( .BOTH. , #1984 ) ;
#15436 = CARTESIAN_POINT ( 'NONE',  ( 38.58424406990784661, 119.9651871740939839, 32.77220824515698183 ) ) ;
#15437 = EDGE_LOOP ( 'NONE', ( #17829, #19510, #17483, #7974 ) ) ;
#15438 = ORIENTED_EDGE ( 'NONE', *, *, #6661, .T. ) ;
#15439 = CARTESIAN_POINT ( 'NONE',  ( 116.4417310231185780, -126.9891397928655010, 30.00000000000000000 ) ) ;
#15440 = ORIENTED_EDGE ( 'NONE', *, *, #17157, .F. ) ;
#15441 = CARTESIAN_POINT ( 'NONE',  ( 46.10157429594899270, 100.7344580088725792, 29.95742577749337343 ) ) ;
#15442 = CARTESIAN_POINT ( 'NONE',  ( 40.27526882409969744, 152.9297705074273210, 30.44471234641812174 ) ) ;
#15443 = CARTESIAN_POINT ( 'NONE',  ( 48.01140435219951996, 155.0604996726487457, 35.83527830041810347 ) ) ;
#15445 = CARTESIAN_POINT ( 'NONE',  ( 61.33076419740685736, 141.3451534613812441, 11.70407797152743079 ) ) ;
#15444 = CARTESIAN_POINT ( 'NONE',  ( 47.43856463449117200, 118.7651871740940237, 32.77220824515698183 ) ) ;
#15446 = CARTESIAN_POINT ( 'NONE',  ( 46.10157429594899270, 71.66049967264873999, 29.95742577749337343 ) ) ;
#15448 = CARTESIAN_POINT ( 'NONE',  ( 41.46631938032478359, 75.38445800887258486, 38.96596240072933170 ) ) ;
#15447 = CARTESIAN_POINT ( 'NONE',  ( 163.4517194221884040, 198.8869265230379995, -5.999999999999976019 ) ) ;
#15449 = EDGE_CURVE ( 'NONE', #12991, #8176, #21199, .T. ) ;
#15450 = CARTESIAN_POINT ( 'NONE',  ( 38.96631938032478359, 123.4104996726487542, 31.27175355779120025 ) ) ;
#15451 = CARTESIAN_POINT ( 'NONE',  ( 47.85071283015097521, 95.37984053634411907, 32.91136586774996431 ) ) ;
#15452 =( BOUNDED_CURVE ( )  B_SPLINE_CURVE ( 2, ( #10865, #12090, #17050, #1962, #19336, #8695, #21110, #12506, #4131, #5992, #7558, #12720, #311 ),
 .UNSPECIFIED., .F., .T. ) 
 B_SPLINE_CURVE_WITH_KNOTS ( ( 3, 2, 2, 2, 2, 2, 3 ),
 ( 0.4779411764705882582, 0.4794117647058823706, 0.4823529411764705954, 0.4852941176470588203, 0.4882352941176470451, 0.4911764705882352700, 0.4926470588235293824 ),
 .UNSPECIFIED. ) 
 CURVE ( )  GEOMETRIC_REPRESENTATION_ITEM ( )  RATIONAL_B_SPLINE_CURVE ( ( 0.9755282581475768211, 0.9755282581475772652, 1.000000000000000000, 0.9510565162951535312, 1.000000000000000000, 0.9510565162951535312, 1.000000000000000000, 0.9510565162951535312, 1.000000000000000000, 0.9510565162951535312, 1.000000000000000000, 0.9755282581475772652, 0.9755282581475768211 ) ) 
 REPRESENTATION_ITEM ( '' )  );
#15453 = CARTESIAN_POINT ( 'NONE',  ( 45.74753988029933538, 74.06518717409399244, 30.44471234641811819 ) ) ;
#15454 = CARTESIAN_POINT ( 'NONE',  ( 47.05648932407426344, 103.9104996726487400, 37.14960608071593384 ) ) ;
#15455 = CARTESIAN_POINT ( 'NONE',  ( -143.8425227516148084, -180.0938272943107279, 44.11586579668791330 ) ) ;
#15456 = CARTESIAN_POINT ( 'NONE',  ( 38.96631938032478359, 133.0104996726487343, 37.14960608071593384 ) ) ;
#15457 = ORIENTED_EDGE ( 'NONE', *, *, #14327, .T. ) ;
#15458 = CARTESIAN_POINT ( 'NONE',  ( -160.8964159109769696, -185.3084106276440082, 46.59394152635518793 ) ) ;
#15459 = CARTESIAN_POINT ( 'NONE',  ( 50.13766412853455279, 153.4730781396112889, -3.927228689826556707 ) ) ;
#15460 = CARTESIAN_POINT ( 'NONE',  ( -159.0959885057557983, -178.8584106276440480, 55.19815736654470584 ) ) ;
#15461 = VERTEX_POINT ( 'NONE', #19760 ) ;
#15462 = CARTESIAN_POINT ( 'NONE',  ( 46.59305225739526435, 139.9151871740940010, 31.60846029578754468 ) ) ;
#15463 = CARTESIAN_POINT ( 'NONE',  ( 38.58424406990786082, 159.1151871740940180, 34.21067981925357060 ) ) ;
#15464 = CARTESIAN_POINT ( 'NONE',  ( 45.74753988029934249, 101.3297705074273267, 30.44471234641812174 ) ) ;
#15465 = CARTESIAN_POINT ( 'NONE',  ( 18.20936163119166196, 143.5026679720446907, 2.934308097026923967 ) ) ;
#15466 = ORIENTED_EDGE ( 'NONE', *, *, #19774, .T. ) ;
#15467 = AXIS2_PLACEMENT_3D ( 'NONE', #370, #4282, #14313 ) ;
#15468 = ORIENTED_EDGE ( 'NONE', *, *, #3630, .F. ) ;
#15469 = CARTESIAN_POINT ( 'NONE',  ( 38.58424406990786082, 111.3797705074273239, 34.21067981925357060 ) ) ;
#15470 = CARTESIAN_POINT ( 'NONE',  ( 38.96631938032478359, 158.4844580088725934, 31.27175355779120025 ) ) ;
#15471 = CARTESIAN_POINT ( 'NONE',  ( 43.01140435219951286, 125.9604996726487514, 29.21067981925356705 ) ) ;
#15472 = CARTESIAN_POINT ( 'NONE',  ( 38.58424406990786082, 141.1151871740939896, 34.21067981925357060 ) ) ;
#15473 = CARTESIAN_POINT ( 'NONE',  ( 43.01140435219951286, 101.9604996726487514, 28.95336869806222779 ) ) ;
#15474 = CARTESIAN_POINT ( 'NONE',  ( 8.944919112598912037, 123.2842988173194385, -4.803623532975393573 ) ) ;
#15475 = EDGE_CURVE ( 'NONE', #3465, #20771, #17870, .T. ) ;
#15476 = CARTESIAN_POINT ( 'NONE',  ( -159.5594255724347761, -173.7891397928654840, 43.77915905869157598 ) ) ;
#15477 = LINE ( 'NONE', #19001, #285 ) ;
#15478 = FACE_OUTER_BOUND ( 'NONE', #1634, .T. ) ;
#15479 = CARTESIAN_POINT ( 'NONE',  ( 44.55648932407425633, 76.61049967264874283, 38.96596240072933170 ) ) ;
#15480 = CARTESIAN_POINT ( 'NONE',  ( 41.64333658814960870, 81.97977050742731819, 38.42115945441014446 ) ) ;
#15481 = CARTESIAN_POINT ( 'NONE',  ( 70.21798013780751546, 127.3226622636268672, -1.629293503064584536 ) ) ;
#15482 = CARTESIAN_POINT ( 'NONE',  ( -142.0420953463935803, -177.5438272943107165, 52.72008163687743831 ) ) ;
#15483 = CARTESIAN_POINT ( 'NONE',  ( 39.42975644700377558, 74.81518717409399244, 31.60846029578754468 ) ) ;
#15484 = LINE ( 'NONE', #17125, #13090 ) ;
#15485 = CARTESIAN_POINT ( 'NONE',  ( -151.4692556286852607, -157.7391397928654726, 59.65701158161632378 ) ) ;
#15486 = VERTEX_POINT ( 'NONE', #17981 ) ;
#15487 = DIRECTION ( 'NONE',  ( -0.000000000000000000, -0.000000000000000000, -1.000000000000000000 ) ) ;
#15488 = CARTESIAN_POINT ( 'NONE',  ( 47.05648932407426344, 122.5104996726487343, 31.27175355779120025 ) ) ;
#15489 = CARTESIAN_POINT ( 'NONE',  ( 41.64333658814960870, 134.7797705074273154, 30.00020018409699318 ) ) ;
#15490 = CARTESIAN_POINT ( 'NONE',  ( 32.43765954726634959, 145.6647664193251615, 11.44158087452429129 ) ) ;
#15491 = ORIENTED_EDGE ( 'NONE', *, *, #15045, .T. ) ;
#15492 = CARTESIAN_POINT ( 'NONE',  ( 44.37947211624943833, 61.27977050742732246, 38.42115945441014446 ) ) ;
#15493 = ORIENTED_EDGE ( 'NONE', *, *, #2798, .F. ) ;
#15494 = CARTESIAN_POINT ( 'NONE',  ( 43.01140435219951286, 133.1297705074273381, 38.86567161673127657 ) ) ;
#15495 = CARTESIAN_POINT ( 'NONE',  ( 15.58850788081759475, 140.2644050767460442, -10.20415289822252980 ) ) ;
#15496 = CARTESIAN_POINT ( 'NONE',  ( -145.2889157411863437, -181.4391397928654612, 58.16351966513671812 ) ) ;
#15497 = CARTESIAN_POINT ( 'NONE',  ( 38.58424406990784661, 60.26518717409400239, 35.64915139335016647 ) ) ;
#15498 = DIRECTION ( 'NONE',  ( -0.9385982292947087080, -0.3450121214752276955, -0.000000000000000000 ) ) ;
#15499 = CARTESIAN_POINT ( 'NONE',  ( -149.8854112254399240, -192.7362167067690564, 59.65701158161632378 ) ) ;
#15500 = CARTESIAN_POINT ( 'NONE',  ( 41.64333658814960870, 93.71518717409401233, 38.42115945441014446 ) ) ;
#15501 = CARTESIAN_POINT ( 'NONE',  ( 38.01140435219952707, 153.8604996726487286, 35.83527830041809636 ) ) ;
#15502 = LINE ( 'NONE', #180, #1948 ) ;
#15503 = CARTESIAN_POINT ( 'NONE',  ( -148.3790856849358306, -171.6630981290893203, 59.16757674456786020 ) ) ;
#15504 = CARTESIAN_POINT ( 'NONE',  ( 0.000000000000000000, 0.000000000000000000, 0.000000000000000000 ) ) ;
#15505 = CARTESIAN_POINT ( 'NONE',  ( 38.96631938032478359, 147.0844580088725877, 37.14960608071593384 ) ) ;
#15506 = CARTESIAN_POINT ( 'NONE',  ( 40.27526882409969033, 114.8297705074273125, 37.97664729208901946 ) ) ;
#15507 = CARTESIAN_POINT ( 'NONE',  ( 64.22416581780682066, 138.6102112617928128, -3.133847767204844370 ) ) ;
#15508 = CARTESIAN_POINT ( 'NONE',  ( 48.01140435219951996, 100.4344580088725678, 32.58608133808903773 ) ) ;
#15509 = CARTESIAN_POINT ( 'NONE',  ( 43.01140435219951286, 102.8651871740940038, 38.86567161673127657 ) ) ;
#15510 = CARTESIAN_POINT ( 'NONE',  ( 43.01140435219951996, 119.9070776186055838, -35.00000000000000000 ) ) ;
#15511 = CARTESIAN_POINT ( 'NONE',  ( 16.16624775068580533, 140.9673012293996237, 10.82561872270659009 ) ) ;
#15512 = CARTESIAN_POINT ( 'NONE',  ( 53.64127281404707048, 146.0262708631457542, 11.34682183016344403 ) ) ;
#15513 = CARTESIAN_POINT ( 'NONE',  ( -70.94676665037202667, 193.0091883945747213, 0.000000000000000000 ) ) ;
#15514 = CARTESIAN_POINT ( 'NONE',  ( 39.42975644700377558, 84.67977050742732104, 36.81289934271958941 ) ) ;
#15515 = EDGE_CURVE ( 'NONE', #3562, #18986, #18093, .T. ) ;
#15516 = CARTESIAN_POINT ( 'NONE',  ( 38.01140435219952707, 77.78445800887259054, 34.21067981925357060 ) ) ;
#15517 = CARTESIAN_POINT ( 'NONE',  ( -148.3790856849358306, -172.5891397928654669, 59.16757674456786020 ) ) ;
#15518 = CARTESIAN_POINT ( 'NONE',  ( 39.92123440845004723, 133.1604996726487400, 38.46393386101376421 ) ) ;
#15520 = CARTESIAN_POINT ( 'NONE',  ( 33.37504612857446773, 87.14074678364892179, -12.34672919366563981 ) ) ;
#15519 = CARTESIAN_POINT ( 'NONE',  ( 47.43856463449117200, 82.76518717409400949, 32.77220824515698183 ) ) ;
#15521 = CARTESIAN_POINT ( 'NONE',  ( -142.0420953463936087, -162.6584106276440593, 49.65701158161630957 ) ) ;
#15522 = CARTESIAN_POINT ( 'NONE',  ( -148.5561028927606344, -177.9938272943107336, 58.62277379824867296 ) ) ;
#15523 = DIRECTION ( 'NONE',  ( 0.000000000000000000, 1.000000000000000000, 0.000000000000000000 ) ) ;
#15524 = DIRECTION ( 'NONE',  ( 1.000000000000000000, 0.000000000000000000, 0.000000000000000000 ) ) ;
#15525 = CARTESIAN_POINT ( 'NONE',  ( 43.01140435219951996, 10.71049967264875491, 34.21067981925357060 ) ) ;
#15526 = DIRECTION ( 'NONE',  ( 1.000000000000000000, 0.000000000000000000, 0.000000000000000000 ) ) ;
#15527 = CARTESIAN_POINT ( 'NONE',  ( 40.27526882409969033, 152.9297705074273210, 30.44471234641811819 ) ) ;
#15528 = CARTESIAN_POINT ( 'NONE',  ( 45.74753988029933538, 106.4297705074273068, 37.97664729208901946 ) ) ;
#15529 = CARTESIAN_POINT ( 'NONE',  ( 18.65831473100296023, 143.8050973582651579, -5.046215916575388150 ) ) ;
#15530 = CARTESIAN_POINT ( 'NONE',  ( 46.59305225739526435, 136.3151871740940351, 36.81289934271958941 ) ) ;
#15531 = CARTESIAN_POINT ( 'NONE',  ( -153.0531000319306258, -189.1622583705452030, 39.65701158161629536 ) ) ;
#15532 = CARTESIAN_POINT ( 'NONE',  ( -160.8964159109769696, -164.1584106276440593, 49.65701158161630957 ) ) ;
#15533 = FACE_OUTER_BOUND ( 'NONE', #13371, .T. ) ;
#15534 = CARTESIAN_POINT ( 'NONE',  ( 38.01409278319488294, 147.7425775668531003, 9.723292677533123651 ) ) ;
#15535 =( NAMED_UNIT ( * ) PLANE_ANGLE_UNIT ( ) SI_UNIT ( $, .RADIAN. ) );
#15536 = CARTESIAN_POINT ( 'NONE',  ( 39.42975644700377558, 111.4151871740940010, 36.81289934271958941 ) ) ;
#15537 = ORIENTED_EDGE ( 'NONE', *, *, #9429, .T. ) ;
#15538 = CARTESIAN_POINT ( 'NONE',  ( -157.6495955161842062, -161.0130981290893146, 41.15050349809589392 ) ) ;
#15539 = ORIENTED_EDGE ( 'NONE', *, *, #15475, .T. ) ;
#15540 = CARTESIAN_POINT ( 'NONE',  ( 48.01140435219951996, 100.4344580088725820, 32.58608133808903773 ) ) ;
#15541 = EDGE_CURVE ( 'NONE', #1664, #19660, #11511, .T. ) ;
#15542 = CIRCLE ( 'NONE', #21547, 10.00000000000000888 ) ;
#15543 = CARTESIAN_POINT ( 'NONE',  ( 41.46631938032478359, 154.3104996726487457, 38.96596240072933170 ) ) ;
#15545 = CARTESIAN_POINT ( 'NONE',  ( 64.38652456388278722, 138.1782414180340197, -15.12506982898978158 ) ) ;
#15544 = CARTESIAN_POINT ( 'NONE',  ( 46.59305225739526435, 115.9151871740940010, 31.60846029578754468 ) ) ;
#15546 = ADVANCED_FACE ( 'NONE', ( #14565 ), #16545, .T. ) ;
#15547 = CARTESIAN_POINT ( 'NONE',  ( 41.46631938032478359, 69.11049967264872862, 29.45539723777780239 ) ) ;
#15549 = CARTESIAN_POINT ( 'NONE',  ( 186.6412678396190472, 201.9535489151380148, 23.27362312593913174 ) ) ;
#15548 = CARTESIAN_POINT ( 'NONE',  ( 44.62520010521203062, 144.8567624833121954, 29.46707291594048783 ) ) ;
#15550 = VECTOR ( 'NONE', #20463, 1000.000000000000000 ) ;
#15551 = CARTESIAN_POINT ( 'NONE',  ( 39.92123440845005433, 123.2604996726487201, 29.95742577749336988 ) ) ;
#15552 = CARTESIAN_POINT ( 'NONE',  ( 47.50469609827003836, 95.31385800265883290, 36.42795439419950299 ) ) ;
#15553 = CARTESIAN_POINT ( 'NONE',  ( 45.74753988029933538, 82.16518717409400097, 37.97664729208901946 ) ) ;
#15554 = CARTESIAN_POINT ( 'NONE',  ( -176.9699209214867608, -126.9891397928655010, 30.00000000000000000 ) ) ;
#15555 = CARTESIAN_POINT ( 'NONE',  ( -151.4692556286852891, -182.6438272943107108, 39.74470866294723947 ) ) ;
#15556 = CARTESIAN_POINT ( 'NONE',  ( -143.8425227516148084, -192.9584106276440423, 55.19815736654470584 ) ) ;
#15557 = ORIENTED_EDGE ( 'NONE', *, *, #618, .T. ) ;
#15558 = CARTESIAN_POINT ( 'NONE',  ( 76.40658810299491677, 127.4365358892444959, 12.33923360994393903 ) ) ;
#15559 = ORIENTED_EDGE ( 'NONE', *, *, #3290, .T. ) ;
#15560 = CARTESIAN_POINT ( 'NONE',  ( 47.43856463449117200, 145.4651871740939839, 35.64915139335016647 ) ) ;
#15561 = VECTOR ( 'NONE', #18675, 999.9999999999998863 ) ;
#15562 = PLANE ( 'NONE',  #17295 ) ;
#15563 = CARTESIAN_POINT ( 'NONE',  ( 45.74753988029934249, 103.4297705074273210, 37.97664729208901235 ) ) ;
#15564 = CARTESIAN_POINT ( 'NONE',  ( 69.27296957579615366, 97.94681810169329594, -0.6368323762655749842 ) ) ;
#15565 = ORIENTED_EDGE ( 'NONE', *, *, #14046, .F. ) ;
#15566 = CARTESIAN_POINT ( 'NONE',  ( 22.10153057061799231, 100.9866247252079745, 1.346821830042071566 ) ) ;
#15567 = ORIENTED_EDGE ( 'NONE', *, *, #12505, .F. ) ;
#15568 = DIRECTION ( 'NONE',  ( 1.000000000000000000, 0.000000000000000000, -0.000000000000000000 ) ) ;
#15569 = CARTESIAN_POINT ( 'NONE',  ( 93.25569916848381524, 126.0916958004080755, 4.000000000000003553 ) ) ;
#15570 = CARTESIAN_POINT ( 'NONE',  ( 45.74753988029933538, 149.0651871740940067, 30.44471234641811819 ) ) ;
#15571 =( BOUNDED_CURVE ( )  B_SPLINE_CURVE ( 2, ( #17708, #2612, #752, #4479, #9466, #16054, #4370, #5922, #15740, #17494, #14189, #2726, #12758 ),
 .UNSPECIFIED., .F., .F. ) 
 B_SPLINE_CURVE_WITH_KNOTS ( ( 3, 2, 2, 2, 2, 2, 3 ),
 ( 0.08088235294117647467, 0.08235294117647058709, 0.08529411764705882582, 0.08823529411764706454, 0.09117647058823528938, 0.09411764705882352811, 0.09558823529411764053 ),
 .UNSPECIFIED. ) 
 CURVE ( )  GEOMETRIC_REPRESENTATION_ITEM ( )  RATIONAL_B_SPLINE_CURVE ( ( 0.9755282581475767101, 0.9755282581475768211, 1.000000000000000000, 0.9510565162951535312, 1.000000000000000000, 0.9510565162951535312, 1.000000000000000000, 0.9510565162951535312, 1.000000000000000000, 0.9510565162951535312, 1.000000000000000000, 0.9755282581475768211, 0.9755282581475767101 ) ) 
 REPRESENTATION_ITEM ( '' )  );
#15572 = CARTESIAN_POINT ( 'NONE',  ( 44.55648932407425633, 97.61049967264874283, 38.96596240072933170 ) ) ;
#15573 = CARTESIAN_POINT ( 'NONE',  ( 50.92548328124963319, 86.60151408976496157, 0.07716523989554470442 ) ) ;
#15574 = CARTESIAN_POINT ( 'NONE',  ( 38.01140435219952707, 60.86049967264873573, 35.83527830041809636 ) ) ;
#15575 = CARTESIAN_POINT ( 'NONE',  ( -141.4692556286852891, -165.9891397928654726, 49.65701158161630957 ) ) ;
#15576 = CARTESIAN_POINT ( 'NONE',  ( -154.5594255724347761, -180.9630981290893033, 59.16757674456785310 ) ) ;
#15577 = CARTESIAN_POINT ( 'NONE',  ( 30.08091612619420729, 88.20954595054467973, -6.232194961517499188 ) ) ;
#15578 = PLANE ( 'NONE',  #2715 ) ;
#15579 = CARTESIAN_POINT ( 'NONE',  ( 41.46631938032478359, 99.38445800887258486, 38.96596240072933170 ) ) ;
#15580 = CARTESIAN_POINT ( 'NONE',  ( 43.01140435219951286, 83.62977050742730967, 29.55568802177586463 ) ) ;
#15581 = CARTESIAN_POINT ( 'NONE',  ( -154.3824083646099439, -175.2938272943107165, 58.62277379824867296 ) ) ;
#15582 = CARTESIAN_POINT ( 'NONE',  ( 39.42975644700377558, 77.81518717409399244, 31.60846029578754468 ) ) ;
#15583 = FACE_OUTER_BOUND ( 'NONE', #4120, .T. ) ;
#15584 = DIRECTION ( 'NONE',  ( 1.000000000000000000, 0.000000000000000000, 0.000000000000000000 ) ) ;
#15585 = VERTEX_POINT ( 'NONE', #1131 ) ;
#15586 = CARTESIAN_POINT ( 'NONE',  ( 43.01140435219951286, 84.53445800887256212, 39.21067981925356349 ) ) ;
#15587 = CARTESIAN_POINT ( 'NONE',  ( 43.01140435219951996, 2.710499672648754466, 34.21067981925357060 ) ) ;
#15588 = CARTESIAN_POINT ( 'NONE',  ( 43.01140435219951286, 130.1297705074273381, 38.86567161673127657 ) ) ;
#15589 = CARTESIAN_POINT ( 'NONE',  ( 25.43708531585104993, 141.8584285267105827, 4.160929998272084873 ) ) ;
#15590 = ORIENTED_EDGE ( 'NONE', *, *, #15168, .F. ) ;
#15591 = CARTESIAN_POINT ( 'NONE',  ( 47.05648932407426344, 73.58445800887257349, 31.27175355779120025 ) ) ;
#15592 = ORIENTED_EDGE ( 'NONE', *, *, #10728, .T. ) ;
#15593 = CARTESIAN_POINT ( 'NONE',  ( 45.74753988029933538, 139.4297705074272926, 37.97664729208901946 ) ) ;
#15594 = CARTESIAN_POINT ( 'NONE',  ( 38.96631938032478359, 100.0104996726487485, 37.14960608071593384 ) ) ;
#15595 = CARTESIAN_POINT ( 'NONE',  ( 43.01140435219951286, 122.0344580088725763, 29.21067981925356705 ) ) ;
#15596 = CARTESIAN_POINT ( 'NONE',  ( 43.01140435219951996, 150.5344580088725763, 39.21067981925356349 ) ) ;
#15597 = CARTESIAN_POINT ( 'NONE',  ( 38.58424406990786082, 102.1151871740940180, 34.21067981925357060 ) ) ;
#15598 = CARTESIAN_POINT ( 'NONE',  ( -148.5561028927606344, -155.7938272943107449, 40.69124936498395328 ) ) ;
#15599 = CARTESIAN_POINT ( 'NONE',  ( 43.01140435219951286, 122.0344580088725763, 29.21067981925356705 ) ) ;
#15600 = CARTESIAN_POINT ( 'NONE',  ( -161.4692556286852607, -157.7130981290893033, 46.40781461928724383 ) ) ;
#15601 = AXIS2_PLACEMENT_3D ( 'NONE', #20306, #14892, #13250 ) ;
#15602 = CARTESIAN_POINT ( 'NONE',  ( 38.01140435219951996, 146.6344580088725991, 32.58608133808903773 ) ) ;
#15603 = CARTESIAN_POINT ( 'NONE',  ( 47.43856463449117200, 116.0297705074273154, 32.77220824515698183 ) ) ;
#15604 = CARTESIAN_POINT ( 'NONE',  ( 14.54084317601859588, 100.7536435603138756, 21.43002817983359876 ) ) ;
#15605 = CARTESIAN_POINT ( 'NONE',  ( 45.43987506541010646, 59.62854787734439554, 30.00461993086704027 ) ) ;
#15606 = CARTESIAN_POINT ( 'NONE',  ( 38.58424406990785371, 111.2651871740939953, 35.64915139335015937 ) ) ;
#15607 = ORIENTED_EDGE ( 'NONE', *, *, #6812, .T. ) ;
#15608 = CARTESIAN_POINT ( 'NONE',  ( 47.05648932407426344, 156.9844580088725934, 37.14960608071593384 ) ) ;
#15609 = CARTESIAN_POINT ( 'NONE',  ( 76.20123706073158587, 111.5182621349952257, -8.137091297256032973 ) ) ;
#15610 = CARTESIAN_POINT ( 'NONE',  ( 28.62772086389876947, 95.65184626908498444, 8.013395860235284829 ) ) ;
#15611 = EDGE_CURVE ( 'NONE', #19361, #17102, #20408, .T. ) ;
#15612 = DIRECTION ( 'NONE',  ( -0.9385982292947088190, -0.3450121214752274179, 0.000000000000000000 ) ) ;
#15613 = CARTESIAN_POINT ( 'NONE',  ( 44.37947211624943833, 74.47977050742731819, 30.00020018409699318 ) ) ;
#15614 = EDGE_LOOP ( 'NONE', ( #1418, #8977, #3237, #5792 ) ) ;
#15615 = CARTESIAN_POINT ( 'NONE',  ( 38.01140435219952707, 62.78445800887258343, 34.21067981925357060 ) ) ;
#15616 = CARTESIAN_POINT ( 'NONE',  ( 43.01140435219951996, 149.9604996726487798, 29.21067981925357060 ) ) ;
#15617 = CARTESIAN_POINT ( 'NONE',  ( 41.46631938032478359, 133.3104996726487457, 38.96596240072933170 ) ) ;
#15619 = CARTESIAN_POINT ( 'NONE',  ( 36.18411527879869993, 86.44273942418264767, -5.442340506565031433 ) ) ;
#15618 = CARTESIAN_POINT ( 'NONE',  ( 47.43856463449117200, 85.46518717409399812, 35.64915139335016647 ) ) ;
#15620 = CARTESIAN_POINT ( 'NONE',  ( -142.0420953463936087, -159.6584106276440593, 49.65701158161630957 ) ) ;
#15621 = CARTESIAN_POINT ( 'NONE',  ( -143.8425227516148084, -180.6938272943107506, 55.19815736654470584 ) ) ;
#15622 = DIRECTION ( 'NONE',  ( 0.000000000000000000, -1.000000000000000000, 0.000000000000000000 ) ) ;
#15623 = DIRECTION ( 'NONE',  ( -0.000000000000000000, -0.000000000000000000, 1.000000000000000000 ) ) ;
#15624 = CARTESIAN_POINT ( 'NONE',  ( 0.000000000000000000, 0.000000000000000000, 0.000000000000000000 ) ) ;
#15625 = DIRECTION ( 'NONE',  ( -0.000000000000000000, -0.000000000000000000, 1.000000000000000000 ) ) ;
#15626 = DIRECTION ( 'NONE',  ( -0.9385982292947087080, -0.3450121214752279730, -0.000000000000000000 ) ) ;
#15627 = CARTESIAN_POINT ( 'NONE',  ( 46.59305225739526435, 142.5797705074273267, 36.81289934271958941 ) ) ;
#15628 = CARTESIAN_POINT ( 'NONE',  ( 41.64333658814960870, 107.7797705074273154, 30.00020018409699318 ) ) ;
#15629 = CARTESIAN_POINT ( 'NONE',  ( 30.90322180743143576, 151.9278386122780375, 10.43433729856376502 ) ) ;
#15630 = CARTESIAN_POINT ( 'NONE',  ( 47.43856463449117911, 133.4651871740940123, 35.64915139335015937 ) ) ;
#15631 = FACE_BOUND ( 'NONE', #12060, .T. ) ;
#15632 = CARTESIAN_POINT ( 'NONE',  ( -142.0420953463935803, -168.8084106276440366, 52.72008163687743831 ) ) ;
#15633 = DIRECTION ( 'NONE',  ( 1.000000000000000000, 0.000000000000000000, 0.000000000000000000 ) ) ;
#15634 = CYLINDRICAL_SURFACE ( 'NONE', #13795, 2.999999999999997780 ) ;
#15635 = AXIS2_PLACEMENT_3D ( 'NONE', #12457, #454, #12020 ) ;
#15636 = CARTESIAN_POINT ( 'NONE',  ( 16.41399813444308364, 129.5198218381110564, 15.55674365125313763 ) ) ;
#15637 = DIRECTION ( 'NONE',  ( 0.000000000000000000, -0.000000000000000000, -1.000000000000000000 ) ) ;
#15638 = CARTESIAN_POINT ( 'NONE',  ( 47.43856463449118621, 112.6151871740939896, 34.21067981925357060 ) ) ;
#15639 = ORIENTED_EDGE ( 'NONE', *, *, #14046, .T. ) ;
#15640 = FACE_OUTER_BOUND ( 'NONE', #20561, .T. ) ;
#15641 = EDGE_CURVE ( 'NONE', #10404, #2985, #16329, .T. ) ;
#15642 = ORIENTED_EDGE ( 'NONE', *, *, #1717, .F. ) ;
#15643 = CARTESIAN_POINT ( 'NONE',  ( 39.92123440845004723, 101.3344580088725735, 29.95742577749337343 ) ) ;
#15644 = CARTESIAN_POINT ( 'NONE',  ( 39.42975644700377558, 147.0797705074273267, 31.60846029578754468 ) ) ;
#15645 = CARTESIAN_POINT ( 'NONE',  ( 47.05648932407426344, 158.5104996726487343, 31.27175355779120025 ) ) ;
#15647 = CARTESIAN_POINT ( 'NONE',  ( 65.77248029998415291, 103.2585056976580091, 13.37079068582577435 ) ) ;
#15646 = CARTESIAN_POINT ( 'NONE',  ( 39.42975644700377558, 119.8151871740940067, 31.60846029578754468 ) ) ;
#15649 = CARTESIAN_POINT ( 'NONE',  ( 46.10157429594899270, 74.66049967264873999, 29.95742577749337343 ) ) ;
#15648 = PRODUCT_DEFINITION ( 'UNKNOWN', '', #12668, #6655 ) ;
#15651 = DIRECTION ( 'NONE',  ( 0.000000000000000000, 1.000000000000000000, 0.000000000000000000 ) ) ;
#15650 = CARTESIAN_POINT ( 'NONE',  ( 38.96631938032478359, 108.0844580088725877, 37.14960608071593384 ) ) ;
#15652 = CARTESIAN_POINT ( 'NONE',  ( 42.21948215057684450, 72.45757658655230671, 39.21067981925355639 ) ) ;
#15653 = CARTESIAN_POINT ( 'NONE',  ( -151.4692556286852607, -191.3130981290892976, 39.65701158161629536 ) ) ;
#15654 = CARTESIAN_POINT ( 'NONE',  ( 47.43856463449117200, 70.46518717409401233, 35.64915139335016647 ) ) ;
#15655 = CYLINDRICAL_SURFACE ( 'NONE', #13800, 5.425037101889737201 ) ;
#15656 = CARTESIAN_POINT ( 'NONE',  ( -157.2955611005346270, -176.3438272943106710, 41.63779006702063867 ) ) ;
#15657 = ADVANCED_FACE ( 'NONE', ( #4657 ), #11372, .T. ) ;
#15658 = ORIENTED_EDGE ( 'NONE', *, *, #19345, .T. ) ;
#15659 = CARTESIAN_POINT ( 'NONE',  ( -157.2955611005346270, -179.6084106276440764, 41.63779006702063867 ) ) ;
#15660 = CARTESIAN_POINT ( 'NONE',  ( 58.01262221917386341, 89.04620360302797621, 5.834872140203966495 ) ) ;
#15661 = VERTEX_POINT ( 'NONE', #16985 ) ;
#15662 = CARTESIAN_POINT ( 'NONE',  ( 43.01140435219951286, 146.3651871740939896, 29.55568802177586463 ) ) ;
#15663 = CARTESIAN_POINT ( 'NONE',  ( -151.4692556286852891, -196.9891397928655010, 49.65701158161630957 ) ) ;
#15664 = ADVANCED_FACE ( 'NONE', ( #5314 ), #16771, .F. ) ;
#15665 = CARTESIAN_POINT ( 'NONE',  ( 47.43856463449117911, 110.0297705074273296, 32.77220824515697473 ) ) ;
#15666 = CARTESIAN_POINT ( 'NONE',  ( 76.81974253126139729, 125.2811442093199616, -1.589308178208348910 ) ) ;
#15667 = ORIENTED_EDGE ( 'NONE', *, *, #21147, .F. ) ;
#15668 = CARTESIAN_POINT ( 'NONE',  ( 55.20039838223064521, 94.47806301326188816, -0.08174959847185196693 ) ) ;
#15669 = EDGE_LOOP ( 'NONE', ( #4913, #20590, #11829, #21101 ) ) ;
#15670 = ADVANCED_FACE ( 'NONE', ( #18436 ), #9957, .T. ) ;
#15671 = CARTESIAN_POINT ( 'NONE',  ( 108.9927164799167372, 227.3511983043831037, 4.000000000000021316 ) ) ;
#15672 = CARTESIAN_POINT ( 'NONE',  ( -56.84366818088135176, 789.5005544000622422, -3.999999999999996447 ) ) ;
#15673 = VECTOR ( 'NONE', #2479, 1000.000000000000000 ) ;
#15674 = CARTESIAN_POINT ( 'NONE',  ( 41.64333658814960870, 147.7151871740940123, 38.42115945441014446 ) ) ;
#15675 = CARTESIAN_POINT ( 'NONE',  ( 38.01140435219952707, 96.71049967264875136, 34.21067981925357060 ) ) ;
#15676 = CARTESIAN_POINT ( 'NONE',  ( 76.79083979644461522, 114.3551126354810492, -1.232281421064668869 ) ) ;
#15677 = CARTESIAN_POINT ( 'NONE',  ( 39.92123440845005433, 60.26049967264872720, 29.95742577749336988 ) ) ;
#15678 = CARTESIAN_POINT ( 'NONE',  ( -161.4692556286852607, -170.3391397928654953, 52.90620854394536821 ) ) ;
#15679 = CARTESIAN_POINT ( 'NONE',  ( 41.46631938032478359, 153.3844580088725991, 38.96596240072933170 ) ) ;
#15680 = UNCERTAINTY_MEASURE_WITH_UNIT (LENGTH_MEASURE( 1.000000000000000082E-05 ), #12211, 'distance_accuracy_value', 'NONE');
#15681 = DIRECTION ( 'NONE',  ( 0.000000000000000000, -1.000000000000000000, 0.000000000000000000 ) ) ;
#15682 = CARTESIAN_POINT ( 'NONE',  ( -161.4692556286852891, -163.4130981290892635, 52.90620854394536821 ) ) ;
#15683 = ORIENTED_EDGE ( 'NONE', *, *, #13428, .T. ) ;
#15684 = CARTESIAN_POINT ( 'NONE',  ( 44.37947211624943833, 83.47977050742731819, 30.00020018409699318 ) ) ;
#15685 = CARTESIAN_POINT ( 'NONE',  ( -142.0420953463935803, -168.2438272943107336, 46.59394152635518793 ) ) ;
#15686 = CARTESIAN_POINT ( 'NONE',  ( 47.43856463449117911, 82.46518717409398391, 35.64915139335015937 ) ) ;
#15687 = DIRECTION ( 'NONE',  ( -0.000000000000000000, -0.000000000000000000, -1.000000000000000000 ) ) ;
#15688 = CARTESIAN_POINT ( 'NONE',  ( 43.01140435219951996, 70.71049967264875136, 34.21067981925357060 ) ) ;
#15689 = VECTOR ( 'NONE', #2806, 1000.000000000000000 ) ;
#15690 = ORIENTED_EDGE ( 'NONE', *, *, #10597, .T. ) ;
#15691 = CARTESIAN_POINT ( 'NONE',  ( 38.01140435219952707, 117.5604996726487315, 32.58608133808903773 ) ) ;
#15692 = EDGE_CURVE ( 'NONE', #14309, #8397, #18864, .T. ) ;
#15693 = DIRECTION ( 'NONE',  ( 0.000000000000000000, 1.000000000000000000, 0.000000000000000000 ) ) ;
#15694 = CARTESIAN_POINT ( 'NONE',  ( 43.01140435219951286, 134.6297705074273097, 29.55568802177586107 ) ) ;
#15695 = CARTESIAN_POINT ( 'NONE',  ( 21.13084688720937976, 146.0403058103794649, -16.94226050084479596 ) ) ;
#15696 = ORIENTED_EDGE ( 'NONE', *, *, #14155, .F. ) ;
#15697 = DIRECTION ( 'NONE',  ( -1.000000000000000000, 0.000000000000000000, 0.000000000000000000 ) ) ;
#15698 =( BOUNDED_CURVE ( )  B_SPLINE_CURVE ( 2, ( #7079, #5407, #19079, #15340, #12240, #17409, #2314, #18970, #12125, #8944, #17085, #554, #18857 ),
 .UNSPECIFIED., .F., .F. ) 
 B_SPLINE_CURVE_WITH_KNOTS ( ( 3, 2, 2, 2, 2, 2, 3 ),
 ( 0.2132352941176470507, 0.2147058823529411631, 0.2176470588235294157, 0.2205882352941176405, 0.2235294117647058931, 0.2264705882352941180, 0.2279411764705882304 ),
 .UNSPECIFIED. ) 
 CURVE ( )  GEOMETRIC_REPRESENTATION_ITEM ( )  RATIONAL_B_SPLINE_CURVE ( ( 0.9755282581475768211, 0.9755282581475768211, 1.000000000000000000, 0.9510565162951535312, 1.000000000000000000, 0.9510565162951535312, 1.000000000000000000, 0.9510565162951535312, 1.000000000000000000, 0.9510565162951535312, 1.000000000000000000, 0.9755282581475768211, 0.9755282581475768211 ) ) 
 REPRESENTATION_ITEM ( '' )  );
#15699 = ORIENTED_EDGE ( 'NONE', *, *, #11424, .T. ) ;
#15700 = CARTESIAN_POINT ( 'NONE',  ( 47.43856463449117200, 139.7297705074273324, 35.64915139335016647 ) ) ;
#15701 = CARTESIAN_POINT ( 'NONE',  ( 40.27526882409969033, 90.82977050742731251, 37.97664729208901946 ) ) ;
#15702 = AXIS2_PLACEMENT_3D ( 'NONE', #5602, #11108, #7495 ) ;
#15703 = CARTESIAN_POINT ( 'NONE',  ( 130.1509106190733007, 127.1041540266590602, -19.99999999999997868 ) ) ;
#15704 = LINE ( 'NONE', #2157, #1836 ) ;
#15705 = CARTESIAN_POINT ( 'NONE',  ( -143.3790856849358306, -194.7630981290893146, 43.77915905869157598 ) ) ;
#15706 = AXIS2_PLACEMENT_3D ( 'NONE', #13512, #8777, #6696 ) ;
#15707 = CARTESIAN_POINT ( 'NONE',  ( 40.27526882409969033, 96.56518717409399244, 37.97664729208901946 ) ) ;
#15708 = CARTESIAN_POINT ( 'NONE',  ( 43.01140435219951286, 65.96049967264873715, 29.21067981925356705 ) ) ;
#15709 = CARTESIAN_POINT ( 'NONE',  ( 48.01140435219951996, 125.3604996726487286, 32.58608133808903773 ) ) ;
#15710 = CARTESIAN_POINT ( 'NONE',  ( -154.5594255724347761, -156.9630981290893317, 59.16757674456785310 ) ) ;
#15711 = DIRECTION ( 'NONE',  ( 0.000000000000000000, 0.000000000000000000, 1.000000000000000000 ) ) ;
#15712 = EDGE_CURVE ( 'NONE', #2417, #13557, #12025, .T. ) ;
#15713 = EDGE_CURVE ( 'NONE', #8428, #1193, #12222, .T. ) ;
#15714 = CARTESIAN_POINT ( 'NONE',  ( 44.55648932407425633, 70.61049967264872862, 38.96596240072933170 ) ) ;
#15715 = CARTESIAN_POINT ( 'NONE',  ( 47.05648932407426344, 129.9844580088725934, 37.14960608071593384 ) ) ;
#15716 = CARTESIAN_POINT ( 'NONE',  ( 44.37947211624943833, 116.4797705074273324, 30.00020018409699318 ) ) ;
#15717 = CARTESIAN_POINT ( 'NONE',  ( 47.04142330690687857, 147.8988775214238842, 10.08059930640748902 ) ) ;
#15718 = CARTESIAN_POINT ( 'NONE',  ( -160.8964159109769696, -191.0438272943107449, 46.59394152635518793 ) ) ;
#15719 = CARTESIAN_POINT ( 'NONE',  ( 38.58424406990786082, 105.1151871740940038, 34.21067981925357060 ) ) ;
#15720 = AXIS2_PLACEMENT_3D ( 'NONE', #17767, #10954, #21100 ) ;
#15721 = EDGE_LOOP ( 'NONE', ( #7637, #6516, #3314, #7927 ) ) ;
#15722 = CARTESIAN_POINT ( 'NONE',  ( 48.01140435219951996, 76.43445800887258201, 32.58608133808903773 ) ) ;
#15723 = CARTESIAN_POINT ( 'NONE',  ( 44.41273964558330789, 85.70220254879866673, -6.708519844216274564 ) ) ;
#15724 = AXIS2_PLACEMENT_3D ( 'NONE', #8673, #15395, #720 ) ;
#15725 = CARTESIAN_POINT ( 'NONE',  ( 23.35610682547305927, 99.68565781958278649, 15.27541961222430444 ) ) ;
#15726 = FACE_OUTER_BOUND ( 'NONE', #252, .T. ) ;
#15727 = CARTESIAN_POINT ( 'NONE',  ( 39.42975644700377558, 78.07977050742731251, 31.60846029578754468 ) ) ;
#15728 = AXIS2_PLACEMENT_3D ( 'NONE', #20777, #2467, #15697 ) ;
#15729 = EDGE_LOOP ( 'NONE', ( #6167, #9534, #12586, #19544 ) ) ;
#15730 = CARTESIAN_POINT ( 'NONE',  ( 48.01140435219951996, 67.28445800887257633, 34.21067981925357060 ) ) ;
#15731 = CARTESIAN_POINT ( 'NONE',  ( -143.3790856849358306, -171.6891397928654897, 43.77915905869157598 ) ) ;
#15732 = CARTESIAN_POINT ( 'NONE',  ( 41.46631938032478359, 123.1104996726487570, 29.45539723777780239 ) ) ;
#15734 = CARTESIAN_POINT ( 'NONE',  ( 76.55129369653414528, 113.4641082036936837, -0.2041528983002713349 ) ) ;
#15733 = CARTESIAN_POINT ( 'NONE',  ( 46.59305225739526435, 79.91518717409400097, 31.60846029578754468 ) ) ;
#15735 = VECTOR ( 'NONE', #1149, 1000.000000000000000 ) ;
#15736 = CARTESIAN_POINT ( 'NONE',  ( -142.0420953463935803, -177.5438272943107165, 52.72008163687743831 ) ) ;
#15737 = CARTESIAN_POINT ( 'NONE',  ( 46.10157429594899270, 113.6604996726487400, 29.95742577749336988 ) ) ;
#15738 = CARTESIAN_POINT ( 'NONE',  ( -159.5594255724347761, -190.8630981290893089, 43.77915905869157598 ) ) ;
#15739 = LINE ( 'NONE', #7161, #11399 ) ;
#15740 = CARTESIAN_POINT ( 'NONE',  ( 38.96631938032478359, 149.4844580088725934, 31.27175355779120025 ) ) ;
#15741 = CARTESIAN_POINT ( 'NONE',  ( 41.64333658814960870, 143.7797705074273154, 30.00020018409699318 ) ) ;
#15742 = CARTESIAN_POINT ( 'NONE',  ( 38.58424406990784661, 108.5297705074273011, 35.64915139335016647 ) ) ;
#15743 = CARTESIAN_POINT ( 'NONE',  ( 9.203281625063985061, 114.5318647093721864, 15.91056058043385413 ) ) ;
#15744 = CARTESIAN_POINT ( 'NONE',  ( 44.37947211624943833, 133.0151871740939953, 38.42115945441014446 ) ) ;
#15745 = CARTESIAN_POINT ( 'NONE',  ( 48.01140435219951996, 67.13445800887257064, 35.83527830041809636 ) ) ;
#15746 = CARTESIAN_POINT ( 'NONE',  ( -157.2955611005345986, -163.7084106276439854, 57.67623309621197336 ) ) ;
#15747 = CARTESIAN_POINT ( 'NONE',  ( -151.4692556286852607, -156.8130981290892692, 59.65701158161632378 ) ) ;
#15748 = DIRECTION ( 'NONE',  ( 0.000000000000000000, 0.000000000000000000, 1.000000000000000000 ) ) ;
#15749 = EDGE_CURVE ( 'NONE', #10293, #20239, #15203, .T. ) ;
#15750 = CARTESIAN_POINT ( 'NONE',  ( 52.07920593110389262, 93.11959619657488929, 13.05671643426689776 ) ) ;
#15751 = AXIS2_PLACEMENT_3D ( 'NONE', #21094, #15681, #14028 ) ;
#15752 = CARTESIAN_POINT ( 'NONE',  ( 46.59305225739526435, 118.9151871740940010, 31.60846029578754468 ) ) ;
#15753 = VERTEX_POINT ( 'NONE', #13683 ) ;
#15754 = FACE_OUTER_BOUND ( 'NONE', #17023, .T. ) ;
#15755 = ORIENTED_EDGE ( 'NONE', *, *, #7748, .T. ) ;
#15756 = CARTESIAN_POINT ( 'NONE',  ( 44.55648932407425633, 88.88445800887258486, 29.45539723777780239 ) ) ;
#15757 = CARTESIAN_POINT ( 'NONE',  ( 46.10157429594899270, 158.6604996726487116, 29.95742577749337343 ) ) ;
#15759 = CARTESIAN_POINT ( 'NONE',  ( 24.14732448757077776, 99.05405632904258084, -4.767757741039170938 ) ) ;
#15758 = CARTESIAN_POINT ( 'NONE',  ( 39.42975644700377558, 111.4151871740940010, 36.81289934271958941 ) ) ;
#15760 = AXIS2_PLACEMENT_3D ( 'NONE', #15510, #1741, #16933 ) ;
#15761 = CARTESIAN_POINT ( 'NONE',  ( 43.01140435219951286, 74.96049967264873715, 28.95336869806222779 ) ) ;
#15763 = DIRECTION ( 'NONE',  ( 0.000000000000000000, 0.000000000000000000, 1.000000000000000000 ) ) ;
#15762 = DIRECTION ( 'NONE',  ( 0.000000000000000000, 0.000000000000000000, 1.000000000000000000 ) ) ;
#15764 = AXIS2_PLACEMENT_3D ( 'NONE', #8225, #1164, #14600 ) ;
#15765 = CARTESIAN_POINT ( 'NONE',  ( -161.4692556286852891, -172.7130981290892748, 46.40781461928724383 ) ) ;
#15766 = CARTESIAN_POINT ( 'NONE',  ( 47.34189385015955054, 95.28487160918048460, 31.70594869545381655 ) ) ;
#15767 = CARTESIAN_POINT ( 'NONE',  ( 47.43856463449118621, 70.61518717409400381, 34.21067981925357060 ) ) ;
#15768 = DIRECTION ( 'NONE',  ( 0.3428981916074309577, -0.9393725726208709270, 0.000000000000000000 ) ) ;
#15769 = CARTESIAN_POINT ( 'NONE',  ( -160.8964159109769696, -181.8938272943107108, 49.65701158161630957 ) ) ;
#15770 = CARTESIAN_POINT ( 'NONE',  ( -145.6429501568359797, -193.1084106276440480, 57.67623309621197336 ) ) ;
#15771 = ORIENTED_EDGE ( 'NONE', *, *, #9090, .F. ) ;
#15772 = CARTESIAN_POINT ( 'NONE',  ( 40.23585178891228509, 85.70481357498144348, 6.429941473113898631 ) ) ;
#15773 = VERTEX_POINT ( 'NONE', #1683 ) ;
#15774 = CARTESIAN_POINT ( 'NONE',  ( 38.58424406990784661, 141.2651871740940237, 35.64915139335016647 ) ) ;
#15775 = CARTESIAN_POINT ( 'NONE',  ( 38.58424406990785371, 156.2651871740939953, 35.64915139335015937 ) ) ;
#15776 = CARTESIAN_POINT ( 'NONE',  ( 38.58424406990785371, 108.2297705074273324, 32.77220824515697473 ) ) ;
#15777 = EDGE_LOOP ( 'NONE', ( #9662, #9773, #21288, #2600 ) ) ;
#15778 = ORIENTED_EDGE ( 'NONE', *, *, #1462, .T. ) ;
#15779 = CARTESIAN_POINT ( 'NONE',  ( 59.83664469576316236, 97.27638873328486113, 6.703993115985443119 ) ) ;
#15780 = ADVANCED_FACE ( 'NONE', ( #20526 ), #5413, .F. ) ;
#15781 = EDGE_LOOP ( 'NONE', ( #19602, #16772, #21372, #10286 ) ) ;
#15782 = CARTESIAN_POINT ( 'NONE',  ( 48.01140435219951996, 89.36049967264874283, 32.58608133808903773 ) ) ;
#15783 = CARTESIAN_POINT ( 'NONE',  ( 47.43856463449117200, 142.7651871740939669, 32.77220824515698183 ) ) ;
#15784 = CARTESIAN_POINT ( 'NONE',  ( 48.01140435219951996, 98.06049967264873146, 35.83527830041810347 ) ) ;
#15785 = CARTESIAN_POINT ( 'NONE',  ( 55.11952973528949684, 87.88698225678692211, -7.065691903092018222 ) ) ;
#15786 = CARTESIAN_POINT ( 'NONE',  ( 136.2768881589198884, 181.8432453435730451, 21.25738000485995016 ) ) ;
#15787 = CARTESIAN_POINT ( 'NONE',  ( -145.2889157411863721, -174.5391397928654840, 41.15050349809590102 ) ) ;
#15788 = CARTESIAN_POINT ( 'NONE',  ( 147.5268905834513475, 193.0332408774651185, -50.99999999999998579 ) ) ;
#15789 = LINE ( 'NONE', #5760, #16950 ) ;
#15790 = VERTEX_POINT ( 'NONE', #20417 ) ;
#15791 = CARTESIAN_POINT ( 'NONE',  ( 38.58424406990784661, 84.52977050742731535, 35.64915139335016647 ) ) ;
#15792 = CARTESIAN_POINT ( 'NONE',  ( -145.6429501568359797, -162.8438272943107279, 57.67623309621198047 ) ) ;
#15793 = CARTESIAN_POINT ( 'NONE',  ( 47.43856463449117911, 67.46518717409399812, 35.64915139335015937 ) ) ;
#15794 = CARTESIAN_POINT ( 'NONE',  ( 54.54805624998882507, 152.1374805055981199, -2.779977617235711129 ) ) ;
#15795 = CARTESIAN_POINT ( 'NONE',  ( -145.6429501568359797, -193.1084106276440480, 57.67623309621198047 ) ) ;
#15796 = ORIENTED_EDGE ( 'NONE', *, *, #16809, .F. ) ;
#15797 = CARTESIAN_POINT ( 'NONE',  ( 43.01140435219951286, 116.9604996726487371, 29.21067981925356705 ) ) ;
#15798 = CARTESIAN_POINT ( 'NONE',  ( 48.01140435219951996, 122.0604996726487315, 35.83527830041809636 ) ) ;
#15799 = CARTESIAN_POINT ( 'NONE',  ( 38.58424406990785371, 132.5297705074272869, 35.64915139335015937 ) ) ;
#15800 = CARTESIAN_POINT ( 'NONE',  ( 17.98086284713512129, 132.6641746743869135, 10.68742175872072409 ) ) ;
#15801 = ORIENTED_EDGE ( 'NONE', *, *, #2549, .T. ) ;
#15802 = VERTEX_POINT ( 'NONE', #10176 ) ;
#15803 = CARTESIAN_POINT ( 'NONE',  ( 45.74753988029933538, 136.4297705074273210, 37.97664729208901946 ) ) ;
#15804 = CARTESIAN_POINT ( 'NONE',  ( 48.01140435219951996, 139.1344580088725706, 35.83527830041809636 ) ) ;
#15805 = CARTESIAN_POINT ( 'NONE',  ( 48.01140435219951996, 155.3604996726487570, 32.58608133808903773 ) ) ;
#15806 = CARTESIAN_POINT ( 'NONE',  ( 38.01140435219952707, 99.56049967264873146, 32.58608133808903773 ) ) ;
#15807 = CARTESIAN_POINT ( 'NONE',  ( 43.80332655382220253, 120.6113394311928460, 39.21067981925355639 ) ) ;
#15808 = CARTESIAN_POINT ( 'NONE',  ( 43.01140435219951996, 10.71049967264875491, 29.21067981925357060 ) ) ;
#15809 = ADVANCED_FACE ( 'NONE', ( #16876 ), #20310, .T. ) ;
#15810 = CARTESIAN_POINT ( 'NONE',  ( 44.37947211624943833, 94.01518717409400949, 38.42115945441014446 ) ) ;
#15811 = CARTESIAN_POINT ( 'NONE',  ( 43.80332655382221674, 132.6113394311928175, 39.21067981925355639 ) ) ;
#15812 = DIRECTION ( 'NONE',  ( 1.000000000000000000, 0.000000000000000000, 0.000000000000000000 ) ) ;
#15813 = CARTESIAN_POINT ( 'NONE',  ( -151.4692556286852891, -155.3130981290892976, 39.14238933923362396 ) ) ;
#15814 = CARTESIAN_POINT ( 'NONE',  ( 43.01140435219951286, 70.46049967264873715, 39.21067981925356349 ) ) ;
#15815 = CARTESIAN_POINT ( 'NONE',  ( 39.92123440845004723, 128.3344580088725877, 29.95742577749337343 ) ) ;
#15816 = CARTESIAN_POINT ( 'NONE',  ( 47.43856463449118621, 112.8797705074273097, 34.21067981925357060 ) ) ;
#15817 = CARTESIAN_POINT ( 'NONE',  ( 46.79023103138236905, 91.88018867020078062, 6.271112617211819007 ) ) ;
#15818 = CARTESIAN_POINT ( 'NONE',  ( -143.8425227516148084, -189.6938272943107222, 55.19815736654470584 ) ) ;
#15819 = CARTESIAN_POINT ( 'NONE',  ( 46.59305225739526435, 97.31518717409400665, 36.81289934271958941 ) ) ;
#15820 = ORIENTED_EDGE ( 'NONE', *, *, #6558, .T. ) ;
#15821 = CARTESIAN_POINT ( 'NONE',  ( 43.80332655382220253, 156.6113394311928744, 39.21067981925355639 ) ) ;
#15822 = CARTESIAN_POINT ( 'NONE',  ( 55.11952973528949684, 87.88698225678692211, -7.065691903092018222 ) ) ;
#15823 =( BOUNDED_CURVE ( )  B_SPLINE_CURVE ( 2, ( #1871, #18736, #3853, #12325, #19060, #5713, #20608, #15745, #6951, #20391, #3963, #12108, #20504 ),
 .UNSPECIFIED., .F., .F. ) 
 B_SPLINE_CURVE_WITH_KNOTS ( ( 3, 2, 2, 2, 2, 2, 3 ),
 ( 0.8897058823529412352, 0.8911764705882353477, 0.8941176470588235725, 0.8970588235294117974, 0.9000000000000000222, 0.9029411764705882470, 0.9044117647058823595 ),
 .UNSPECIFIED. ) 
 CURVE ( )  GEOMETRIC_REPRESENTATION_ITEM ( )  RATIONAL_B_SPLINE_CURVE ( ( 0.9755282581475768211, 0.9755282581475777093, 1.000000000000000000, 0.9510565162951535312, 1.000000000000000000, 0.9510565162951535312, 1.000000000000000000, 0.9510565162951535312, 1.000000000000000000, 0.9510565162951535312, 1.000000000000000000, 0.9755282581475768211, 0.9755282581475768211 ) ) 
 REPRESENTATION_ITEM ( '' )  );
#15824 = CARTESIAN_POINT ( 'NONE',  ( 33.01799438418878907, 146.2770090272405810, 10.51364782838779099 ) ) ;
#15825 = PLANE ( 'NONE',  #12146 ) ;
#15826 = AXIS2_PLACEMENT_3D ( 'NONE', #5257, #1947, #8678 ) ;
#15827 = CARTESIAN_POINT ( 'NONE',  ( 38.58424406990785371, 72.22977050742731819, 32.77220824515697473 ) ) ;
#15828 = EDGE_LOOP ( 'NONE', ( #11714, #3514, #3289, #18695 ) ) ;
#15829 = ORIENTED_EDGE ( 'NONE', *, *, #6074, .T. ) ;
#15830 = EDGE_CURVE ( 'NONE', #14246, #15135, #8524, .T. ) ;
#15831 = EDGE_CURVE ( 'NONE', #5848, #18715, #5694, .T. ) ;
#15832 = LINE ( 'NONE', #5585, #11585 ) ;
#15833 = CARTESIAN_POINT ( 'NONE',  ( 47.05648932407426344, 115.9104996726487400, 37.14960608071593384 ) ) ;
#15835 = CARTESIAN_POINT ( 'NONE',  ( 35.49642027120339094, 86.59030162945495590, 1.581590266896775843 ) ) ;
#15834 = CARTESIAN_POINT ( 'NONE',  ( 44.37947211624943833, 76.01518717409399528, 38.42115945441014446 ) ) ;
#15836 = CARTESIAN_POINT ( 'NONE',  ( -145.6429501568359797, -167.9438272943107222, 41.63779006702063867 ) ) ;
#15837 = CARTESIAN_POINT ( 'NONE',  ( 15.97061701817242785, 140.8453463817331794, 16.82122940411608170 ) ) ;
#15838 = CARTESIAN_POINT ( 'NONE',  ( -161.4692556286853176, -184.5630981290892976, 49.65701158161630957 ) ) ;
#15839 = DIRECTION ( 'NONE',  ( 0.000000000000000000, 1.000000000000000000, 0.000000000000000000 ) ) ;
#15840 = CYLINDRICAL_SURFACE ( 'NONE', #11055, 7.500000000000000000 ) ;
#15841 = CARTESIAN_POINT ( 'NONE',  ( 44.55648932407425633, 157.8844580088725706, 29.45539723777780239 ) ) ;
#15842 = CARTESIAN_POINT ( 'NONE',  ( 45.74753988029933538, 143.3297705074272699, 30.44471234641811819 ) ) ;
#15843 = CARTESIAN_POINT ( 'NONE',  ( 61.83586340360074018, 91.21788411573329824, -1.307985002297802568 ) ) ;
#15844 = CARTESIAN_POINT ( 'NONE',  ( 44.37947211624943833, 139.0151871740939953, 38.42115945441014446 ) ) ;
#15845 = DIRECTION ( 'NONE',  ( 0.9387810623359077455, 0.3426822732243068881, 0.03548206049944094276 ) ) ;
#15846 = CARTESIAN_POINT ( 'NONE',  ( -151.4692556286852891, -164.9084106276440593, 39.74470866294723947 ) ) ;
#15847 = DIRECTION ( 'NONE',  ( 0.000000000000000000, 0.000000000000000000, 1.000000000000000000 ) ) ;
#15848 = DIRECTION ( 'NONE',  ( 1.000000000000000000, 0.000000000000000000, 0.000000000000000000 ) ) ;
#15849 = CARTESIAN_POINT ( 'NONE',  ( 49.77943037783704483, 92.44786530929899016, 6.152137702922222395 ) ) ;
#15850 = PLANE ( 'NONE',  #1794 ) ;
#15851 = CARTESIAN_POINT ( 'NONE',  ( 47.43856463449117200, 112.4651871740939839, 35.64915139335016647 ) ) ;
#15852 = ORIENTED_EDGE ( 'NONE', *, *, #6294, .T. ) ;
#15853 = EDGE_CURVE ( 'NONE', #10538, #119, #11701, .T. ) ;
#15854 = CIRCLE ( 'NONE', #6359, 10.00000000000000888 ) ;
#15855 = EDGE_CURVE ( 'NONE', #2386, #15106, #17293, .T. ) ;
#15856 = CARTESIAN_POINT ( 'NONE',  ( -159.5594255724347761, -179.7891397928654840, 43.77915905869157598 ) ) ;
#15857 = ORIENTED_EDGE ( 'NONE', *, *, #17825, .F. ) ;
#15858 = CARTESIAN_POINT ( 'NONE',  ( 47.05648932407426344, 91.58445800887257349, 31.27175355779120025 ) ) ;
#15859 = CARTESIAN_POINT ( 'NONE',  ( 39.92123440845004723, 145.1604996726487116, 38.46393386101376421 ) ) ;
#15861 = CARTESIAN_POINT ( 'NONE',  ( 22.77429378292968920, 139.4308542021594519, -2.981927144630473148 ) ) ;
#15860 = CARTESIAN_POINT ( 'NONE',  ( 41.64333658814960870, 102.7151871740939981, 38.42115945441014446 ) ) ;
#15862 = CARTESIAN_POINT ( 'NONE',  ( 44.55648932407425633, 67.61049967264872862, 38.96596240072933170 ) ) ;
#15864 = CARTESIAN_POINT ( 'NONE',  ( 43.01140435219951996, 148.4604996726487798, 39.21067981925356349 ) ) ;
#15863 = CARTESIAN_POINT ( 'NONE',  ( 43.01140435219951996, 10.71049967264875491, 29.21067981925357060 ) ) ;
#15865 = SURFACE_STYLE_FILL_AREA ( #2315 ) ;
#15866 = DIRECTION ( 'NONE',  ( -0.000000000000000000, -0.000000000000000000, -1.000000000000000000 ) ) ;
#15867 = DIRECTION ( 'NONE',  ( -0.000000000000000000, -0.000000000000000000, 1.000000000000000000 ) ) ;
#15868 = LINE ( 'NONE', #20956, #14690 ) ;
#15869 = CARTESIAN_POINT ( 'NONE',  ( -160.8964159109769696, -170.0438272943107449, 46.59394152635518793 ) ) ;
#15870 = CARTESIAN_POINT ( 'NONE',  ( -145.6429501568359797, -192.2084106276440139, 41.63779006702063867 ) ) ;
#15871 = VERTEX_POINT ( 'NONE', #11924 ) ;
#15872 = CARTESIAN_POINT ( 'NONE',  ( -145.6429501568359797, -177.2084106276440423, 41.63779006702063867 ) ) ;
#15873 = CARTESIAN_POINT ( 'NONE',  ( 11.68597903420391226, 105.9017562933008918, 7.620467510411443435 ) ) ;
#15874 = CARTESIAN_POINT ( 'NONE',  ( 39.42975644700377558, 144.4151871740940294, 36.81289934271958941 ) ) ;
#15875 = CARTESIAN_POINT ( 'NONE',  ( 41.64333658814960870, 155.5151871740940237, 30.00020018409699318 ) ) ;
#15876 = CARTESIAN_POINT ( 'NONE',  ( 45.74753988029934249, 104.3297705074273125, 30.44471234641812174 ) ) ;
#15877 = EDGE_LOOP ( 'NONE', ( #3804, #11272, #9009, #9129 ) ) ;
#15878 = VERTEX_POINT ( 'NONE', #18653 ) ;
#15879 = CARTESIAN_POINT ( 'NONE',  ( 71.16904767199986281, 118.3707548728134213, -1.272037577920760665 ) ) ;
#15880 =( BOUNDED_CURVE ( )  B_SPLINE_CURVE ( 2, ( #4708, #14412, #16385, #11426, #6033, #1298, #6366, #2732, #14520, #13091, #9472, #19818, #1083 ),
 .UNSPECIFIED., .F., .F. ) 
 B_SPLINE_CURVE_WITH_KNOTS ( ( 3, 2, 2, 2, 2, 2, 3 ),
 ( 0.08088235294117646079, 0.08235294117647058709, 0.08529411764705882582, 0.08823529411764706454, 0.09117647058823528938, 0.09411764705882352811, 0.09558823529411765441 ),
 .UNSPECIFIED. ) 
 CURVE ( )  GEOMETRIC_REPRESENTATION_ITEM ( )  RATIONAL_B_SPLINE_CURVE ( ( 0.9755282581475767101, 0.9755282581475765991, 1.000000000000000000, 0.9510565162951535312, 1.000000000000000000, 0.9510565162951535312, 1.000000000000000000, 0.9510565162951535312, 1.000000000000000000, 0.9510565162951535312, 1.000000000000000000, 0.9755282581475765991, 0.9755282581475767101 ) ) 
 REPRESENTATION_ITEM ( '' )  );
#15881 = ORIENTED_EDGE ( 'NONE', *, *, #13466, .T. ) ;
#15882 = CARTESIAN_POINT ( 'NONE',  ( 47.05648932407426344, 115.5844580088725877, 31.27175355779120025 ) ) ;
#15883 = CARTESIAN_POINT ( 'NONE',  ( 43.01140435219951286, 89.96049967264873715, 29.21067981925356705 ) ) ;
#15884 = CARTESIAN_POINT ( 'NONE',  ( 38.58424406990786082, 75.37977050742732388, 34.21067981925357060 ) ) ;
#15885 = CARTESIAN_POINT ( 'NONE',  ( 38.58424406990784661, 135.2651871740939953, 35.64915139335016647 ) ) ;
#15886 = CARTESIAN_POINT ( 'NONE',  ( 41.46631938032478359, 102.1104996726487286, 29.45539723777780239 ) ) ;
#15887 = CARTESIAN_POINT ( 'NONE',  ( 77.22939692449374149, 120.9137088693742044, 5.553548964694690504 ) ) ;
#15888 = CARTESIAN_POINT ( 'NONE',  ( 43.80332655382220253, 119.8836182503284533, 29.21067981925356705 ) ) ;
#15889 = CARTESIAN_POINT ( 'NONE',  ( -151.4692556286852891, -157.7391397928654442, 60.17163382399899518 ) ) ;
#15890 = CARTESIAN_POINT ( 'NONE',  ( 38.96631938032478359, 153.0844580088725877, 37.14960608071593384 ) ) ;
#15891 = CARTESIAN_POINT ( 'NONE',  ( 43.80332655382220253, 63.61133943119283174, 39.21067981925355639 ) ) ;
#15892 = VECTOR ( 'NONE', #7224, 1000.000000000000000 ) ;
#15893 = VECTOR ( 'NONE', #10858, 1000.000000000000000 ) ;
#15894 = ORIENTED_EDGE ( 'NONE', *, *, #16496, .T. ) ;
#15895 = CARTESIAN_POINT ( 'NONE',  ( 43.01140435219951286, 86.62977050742730967, 29.55568802177586463 ) ) ;
#15896 = CARTESIAN_POINT ( 'NONE',  ( -151.4692556286852891, -169.1438272943107108, 59.56931450028537967 ) ) ;
#15897 = CARTESIAN_POINT ( 'NONE',  ( 8.779377865064803999, 119.6051361893432130, -4.922546661887801100 ) ) ;
#15898 = CARTESIAN_POINT ( 'NONE',  ( -160.8964159109769696, -191.1584106276440593, 49.65701158161630957 ) ) ;
#15899 = AXIS2_PLACEMENT_3D ( 'NONE', #14830, #19920, #4697 ) ;
#15900 = VERTEX_POINT ( 'NONE', #10281 ) ;
#15901 = CARTESIAN_POINT ( 'NONE',  ( -153.0531000319306827, -174.8899795514095672, 59.65701158161631668 ) ) ;
#15902 = DIRECTION ( 'NONE',  ( 0.000000000000000000, 1.000000000000000000, 0.000000000000000000 ) ) ;
#15903 = CARTESIAN_POINT ( 'NONE',  ( 41.64333658814960870, 132.9797705074273324, 38.42115945441014446 ) ) ;
#15904 = CARTESIAN_POINT ( 'NONE',  ( 60.78979090282389564, 90.74622564588611340, -6.275468401765792237 ) ) ;
#15905 = ORIENTED_EDGE ( 'NONE', *, *, #13099, .F. ) ;
#15906 = CARTESIAN_POINT ( 'NONE',  ( 44.55648932407425633, 72.68445800887258201, 38.96596240072933170 ) ) ;
#15907 = EDGE_LOOP ( 'NONE', ( #20849, #16836, #4414, #10926 ) ) ;
#15908 = CARTESIAN_POINT ( 'NONE',  ( 38.58424406990784661, 126.2297705074273040, 32.77220824515698183 ) ) ;
#15909 = CARTESIAN_POINT ( 'NONE',  ( 47.05648932407426344, 139.5844580088725877, 31.27175355779120025 ) ) ;
#15910 =( GEOMETRIC_REPRESENTATION_CONTEXT ( 3 ) GLOBAL_UNCERTAINTY_ASSIGNED_CONTEXT ( ( #18781 ) ) GLOBAL_UNIT_ASSIGNED_CONTEXT ( ( #10190, #13586, #13696 ) ) REPRESENTATION_CONTEXT ( 'NONE', 'WORKASPACE' ) );
#15911 = ADVANCED_FACE ( 'NONE', ( #7628 ), #19193, .T. ) ;
#15912 = CARTESIAN_POINT ( 'NONE',  ( 46.10157429594899270, 154.7604996726487343, 38.46393386101375711 ) ) ;
#15913 = CARTESIAN_POINT ( 'NONE',  ( 43.01140435219954838, 110.0344580088725763, 29.21067981925356705 ) ) ;
#15914 = CARTESIAN_POINT ( 'NONE',  ( 162.0641828542163125, 116.7231784796025948, 4.000000000000021316 ) ) ;
#15915 = CARTESIAN_POINT ( 'NONE',  ( -141.4692556286852891, -192.0630981290892976, 49.65701158161630957 ) ) ;
#15916 = CARTESIAN_POINT ( 'NONE',  ( 43.01140435219951286, 99.86518717409400381, 38.86567161673127657 ) ) ;
#15917 = CARTESIAN_POINT ( 'NONE',  ( 43.01140435219951286, 74.96049967264873715, 29.21067981925356705 ) ) ;
#15918 = CYLINDRICAL_SURFACE ( 'NONE', #1960, 10.00000000000000888 ) ;
#15919 = CARTESIAN_POINT ( 'NONE',  ( -148.3790856849358306, -158.4630981290893317, 40.14644641866477315 ) ) ;
#15920 = DIRECTION ( 'NONE',  ( 0.000000000000000000, -1.000000000000000000, 0.000000000000000000 ) ) ;
#15921 = SHAPE_REPRESENTATION ( 'Upper Movable Curved Shear Blade', ( #12657 ), #7037 ) ;
#15922 = CARTESIAN_POINT ( 'NONE',  ( 48.01140435219951996, 133.2844580088726048, 34.21067981925357060 ) ) ;
#15923 = CARTESIAN_POINT ( 'NONE',  ( 40.27526882409969033, 111.8297705074272983, 37.97664729208901946 ) ) ;
#15924 = CARTESIAN_POINT ( 'NONE',  ( 14.90453237821946253, 123.0362832886413855, 8.294721248935834623 ) ) ;
#15925 = CARTESIAN_POINT ( 'NONE',  ( -160.8964159109769696, -190.7438272943107336, 52.72008163687743121 ) ) ;
#15926 = CARTESIAN_POINT ( 'NONE',  ( 43.01140435219951286, 93.86518717409401802, 38.86567161673127657 ) ) ;
#15927 = CARTESIAN_POINT ( 'NONE',  ( 39.92123440845005433, 91.16049967264873999, 38.46393386101375711 ) ) ;
#15928 = EDGE_LOOP ( 'NONE', ( #21542, #1503, #14331, #14906 ) ) ;
#15929 = CARTESIAN_POINT ( 'NONE',  ( 43.01140435219951286, 129.5344580088725763, 39.21067981925356349 ) ) ;
#15930 = EDGE_CURVE ( 'NONE', #9805, #9751, #2172, .T. ) ;
#15931 = CARTESIAN_POINT ( 'NONE',  ( 57.78275410301085913, 89.02518083909171764, -0.1607367497116551913 ) ) ;
#15932 = CARTESIAN_POINT ( 'NONE',  ( 16.56453993303484395, 129.6948329502664308, 9.561135973024818213 ) ) ;
#15933 = DIRECTION ( 'NONE',  ( 0.7066505893342460709, 0.7066505893340065958, 0.03591502732094191408 ) ) ;
#15934 = CARTESIAN_POINT ( 'NONE',  ( 40.27526882409969744, 78.82977050742729830, 37.97664729208901235 ) ) ;
#15935 = ORIENTED_EDGE ( 'NONE', *, *, #21350, .T. ) ;
#15936 = EDGE_CURVE ( 'NONE', #11479, #5662, #9272, .T. ) ;
#15937 = ORIENTED_EDGE ( 'NONE', *, *, #19450, .T. ) ;
#15938 = CARTESIAN_POINT ( 'NONE',  ( 45.74753988029933538, 157.4297705074273495, 37.97664729208901946 ) ) ;
#15939 = CARTESIAN_POINT ( 'NONE',  ( -46.09493621325655255, 160.7104996726487798, -19.99999999999997158 ) ) ;
#15940 = EDGE_CURVE ( 'NONE', #8905, #6932, #14330, .T. ) ;
#15941 = CARTESIAN_POINT ( 'NONE',  ( 46.10157429594899270, 121.7604996726487485, 38.46393386101376421 ) ) ;
#15943 = CARTESIAN_POINT ( 'NONE',  ( 10.18435502709129103, 110.4832086711448227, 2.772112504659519416 ) ) ;
#15942 = CARTESIAN_POINT ( 'NONE',  ( 47.43856463449117200, 73.76518717409399528, 32.77220824515698183 ) ) ;
#15944 = CARTESIAN_POINT ( 'NONE',  ( -143.8425227516148084, -171.6938272943107222, 55.19815736654470584 ) ) ;
#15945 = CARTESIAN_POINT ( 'NONE',  ( 30.90322180743143576, 151.9278386122780375, 10.43433729856376502 ) ) ;
#15946 = CARTESIAN_POINT ( 'NONE',  ( -154.5594255724347761, -185.1630981290893203, 40.14644641866476604 ) ) ;
#15947 = LINE ( 'NONE', #11100, #21635 ) ;
#15948 = CARTESIAN_POINT ( 'NONE',  ( -145.2889157411863437, -163.4391397928654897, 58.16351966513671812 ) ) ;
#15949 = CARTESIAN_POINT ( 'NONE',  ( 41.64333658814960870, 141.9797705074273324, 38.42115945441014446 ) ) ;
#15950 =( BOUNDED_CURVE ( )  B_SPLINE_CURVE ( 2, ( #2110, #12129, #3769, #14003, #5513, #17521, #4088, #12460, #20737, #5411, #10924, #5626, #20846 ),
 .UNSPECIFIED., .F., .F. ) 
 B_SPLINE_CURVE_WITH_KNOTS ( ( 3, 2, 2, 2, 2, 2, 3 ),
 ( 0.9338235294117647189, 0.9352941176470588314, 0.9382352941176470562, 0.9411764705882352811, 0.9441176470588235059, 0.9470588235294117307, 0.9485294117647058432 ),
 .UNSPECIFIED. ) 
 CURVE ( )  GEOMETRIC_REPRESENTATION_ITEM ( )  RATIONAL_B_SPLINE_CURVE ( ( 0.9755282581475768211, 0.9755282581475768211, 1.000000000000000000, 0.9510565162951535312, 1.000000000000000000, 0.9510565162951535312, 1.000000000000000000, 0.9510565162951535312, 1.000000000000000000, 0.9510565162951535312, 1.000000000000000000, 0.9755282581475768211, 0.9755282581475768211 ) ) 
 REPRESENTATION_ITEM ( '' )  );
#15951 = CARTESIAN_POINT ( 'NONE',  ( 45.74753988029934249, 130.1651871740940010, 37.97664729208901235 ) ) ;
#15952 = PLANE ( 'NONE',  #6130 ) ;
#15953 = CARTESIAN_POINT ( 'NONE',  ( -143.8425227516148084, -162.3584106276440480, 44.11586579668791330 ) ) ;
#15954 = PLANE ( 'NONE',  #14995 ) ;
#15955 = DIRECTION ( 'NONE',  ( -1.000000000000000000, 0.000000000000000000, 0.000000000000000000 ) ) ;
#15956 = CARTESIAN_POINT ( 'NONE',  ( 54.90439719837324617, 94.24896709312837118, 12.93774216356182372 ) ) ;
#15957 = CARTESIAN_POINT ( 'NONE',  ( 43.01140435219951286, 121.4604996726487371, 39.21067981925356349 ) ) ;
#15958 = CARTESIAN_POINT ( 'NONE',  ( 43.01140435219951286, 102.8651871740940038, 38.86567161673127657 ) ) ;
#15959 = ADVANCED_FACE ( 'NONE', ( #559 ), #5843, .F. ) ;
#15960 = VERTEX_POINT ( 'NONE', #20848 ) ;
#15961 = CARTESIAN_POINT ( 'NONE',  ( 47.05648932407426344, 86.51049967264874851, 31.27175355779120025 ) ) ;
#15962 = ORIENTED_EDGE ( 'NONE', *, *, #3722, .F. ) ;
#15963 = CARTESIAN_POINT ( 'NONE',  ( 38.01140435219951996, 89.93445800887256780, 35.83527830041810347 ) ) ;
#15964 = CARTESIAN_POINT ( 'NONE',  ( 47.05648932407426344, 148.9104996726487400, 37.14960608071593384 ) ) ;
#15966 = CARTESIAN_POINT ( 'NONE',  ( 64.45983652262509622, 101.7220219035630748, -6.553643814208265361 ) ) ;
#15965 = CARTESIAN_POINT ( 'NONE',  ( 44.37947211624943833, 107.2151871740940123, 30.00020018409699318 ) ) ;
#15967 = EDGE_CURVE ( 'NONE', #19941, #7201, #10817, .T. ) ;
#15968 = DIRECTION ( 'NONE',  ( 0.000000000000000000, 1.000000000000000000, 0.000000000000000000 ) ) ;
#15970 = CARTESIAN_POINT ( 'NONE',  ( -161.4692556286852891, -157.7130981290893033, 46.40781461928724383 ) ) ;
#15969 = CARTESIAN_POINT ( 'NONE',  ( -153.0531000319306827, -167.2362167067690280, 39.65701158161629536 ) ) ;
#15971 = CARTESIAN_POINT ( 'NONE',  ( 48.01140435219951996, 118.2844580088725763, 34.21067981925357060 ) ) ;
#15972 = DIRECTION ( 'NONE',  ( 0.4999999999999996114, 0.000000000000000000, 0.8660254037844388186 ) ) ;
#15973 = DIRECTION ( 'NONE',  ( 1.000000000000000000, 0.000000000000000000, -1.915514545828640458E-16 ) ) ;
#15974 = CARTESIAN_POINT ( 'NONE',  ( 40.27526882409969033, 68.66518717409400097, 30.44471234641811819 ) ) ;
#15975 = CARTESIAN_POINT ( 'NONE',  ( 18.86674891209846905, 143.9013856721611546, -11.04182128657428485 ) ) ;
#15976 = CARTESIAN_POINT ( 'NONE',  ( 46.10157429594899270, 94.76049967264873430, 38.46393386101375711 ) ) ;
#15977 = CARTESIAN_POINT ( 'NONE',  ( -145.6429501568359797, -167.9438272943107506, 41.63779006702063867 ) ) ;
#15978 = CARTESIAN_POINT ( 'NONE',  ( -154.3824083646099439, -191.7584106276440536, 40.69124936498395328 ) ) ;
#15979 = EDGE_LOOP ( 'NONE', ( #6850, #16148, #15820, #16646 ) ) ;
#15980 = CARTESIAN_POINT ( 'NONE',  ( -154.3824083646099439, -176.7584106276440536, 40.69124936498395328 ) ) ;
#15981 = CARTESIAN_POINT ( 'NONE',  ( 30.25101221841200427, 88.05347211559326581, -0.2365872832861977970 ) ) ;
#15982 = ORIENTED_EDGE ( 'NONE', *, *, #15195, .T. ) ;
#15983 = CARTESIAN_POINT ( 'NONE',  ( 38.58424406990784661, 131.9651871740939555, 32.77220824515698183 ) ) ;
#15984 = CARTESIAN_POINT ( 'NONE',  ( 40.27526882409969744, 96.82977050742731251, 37.97664729208901235 ) ) ;
#15985 = ORIENTED_EDGE ( 'NONE', *, *, #11809, .T. ) ;
#15986 = ORIENTED_EDGE ( 'NONE', *, *, #15154, .F. ) ;
#15987 = CARTESIAN_POINT ( 'NONE',  ( 56.80456144658707274, 95.31062238922963559, 13.84685026556700116 ) ) ;
#15988 = ORIENTED_EDGE ( 'NONE', *, *, #12026, .T. ) ;
#15989 = CARTESIAN_POINT ( 'NONE',  ( 47.05648932407426344, 111.9844580088725792, 37.14960608071593384 ) ) ;
#15990 = AXIS2_PLACEMENT_3D ( 'NONE', #10333, #18598, #20362 ) ;
#15991 = CARTESIAN_POINT ( 'NONE',  ( 41.46631938032478359, 76.31049967264874567, 38.96596240072933170 ) ) ;
#15992 = CARTESIAN_POINT ( 'NONE',  ( 40.27526882409969033, 75.82977050742731251, 37.97664729208901946 ) ) ;
#15993 = CARTESIAN_POINT ( 'NONE',  ( 38.58424406990784661, 131.9651871740939555, 32.77220824515698183 ) ) ;
#15994 = CARTESIAN_POINT ( 'NONE',  ( 48.01140435219951996, 92.21049967264873715, 34.21067981925357060 ) ) ;
#15995 = CARTESIAN_POINT ( 'NONE',  ( 77.07719282571002850, 116.5297446719512209, 12.69640610750513865 ) ) ;
#15996 = CARTESIAN_POINT ( 'NONE',  ( 147.5268905834513475, 193.0332408774651185, -50.99999999999998579 ) ) ;
#15997 = CARTESIAN_POINT ( 'NONE',  ( -159.5594255724347761, -161.1891397928654897, 55.53486410454104316 ) ) ;
#15998 = DIRECTION ( 'NONE',  ( 0.000000000000000000, 0.000000000000000000, 1.000000000000000000 ) ) ;
#15999 = ADVANCED_FACE ( 'NONE', ( #2947 ), #4375, .T. ) ;
#16000 = CARTESIAN_POINT ( 'NONE',  ( 43.01140435219951996, 10.71049967264875491, 29.21067981925357060 ) ) ;
#16001 = CARTESIAN_POINT ( 'NONE',  ( -153.0531000319307111, -162.8899795514095672, 59.65701158161632378 ) ) ;
#16002 = VERTEX_POINT ( 'NONE', #16060 ) ;
#16003 = CARTESIAN_POINT ( 'NONE',  ( 39.42975644700377558, 75.07977050742731251, 31.60846029578754468 ) ) ;
#16004 = CARTESIAN_POINT ( 'NONE',  ( 30.08091612619420729, 88.20954595054467973, -6.232194961517499188 ) ) ;
#16005 = FACE_OUTER_BOUND ( 'NONE', #764, .T. ) ;
#16006 = ORIENTED_EDGE ( 'NONE', *, *, #20810, .F. ) ;
#16007 = FACE_BOUND ( 'NONE', #4328, .T. ) ;
#16008 = CARTESIAN_POINT ( 'NONE',  ( 46.10157429594899270, 124.7344580088725934, 29.95742577749336988 ) ) ;
#16009 =( BOUNDED_CURVE ( )  B_SPLINE_CURVE ( 2, ( #12833, #19668, #9433, #9649, #9318, #16136, #1259, #19781, #8101, #6441, #7996, #21550, #21223 ),
 .UNSPECIFIED., .F., .F. ) 
 B_SPLINE_CURVE_WITH_KNOTS ( ( 3, 2, 2, 2, 2, 2, 3 ),
 ( 0.6102941176470587648, 0.6117647058823529882, 0.6147058823529412130, 0.6176470588235294379, 0.6205882352941176627, 0.6235294117647058876, 0.6250000000000000000 ),
 .UNSPECIFIED. ) 
 CURVE ( )  GEOMETRIC_REPRESENTATION_ITEM ( )  RATIONAL_B_SPLINE_CURVE ( ( 0.9755282581475768211, 0.9755282581475758219, 1.000000000000000000, 0.9510565162951535312, 1.000000000000000000, 0.9510565162951535312, 1.000000000000000000, 0.9510565162951535312, 1.000000000000000000, 0.9510565162951535312, 1.000000000000000000, 0.9755282581475768211, 0.9755282581475768211 ) ) 
 REPRESENTATION_ITEM ( '' )  );
#16010 = CARTESIAN_POINT ( 'NONE',  ( 46.59305225739526435, 127.5797705074273267, 36.81289934271958941 ) ) ;
#16011 = EDGE_LOOP ( 'NONE', ( #16474, #8039, #18133, #10608 ) ) ;
#16012 = AXIS2_PLACEMENT_3D ( 'NONE', #6601, #17154, #15298 ) ;
#16013 = CARTESIAN_POINT ( 'NONE',  ( 138.5268905834513191, 193.0332408774651185, -50.99999999999998579 ) ) ;
#16014 = ORIENTED_EDGE ( 'NONE', *, *, #5010, .F. ) ;
#16015 = CARTESIAN_POINT ( 'NONE',  ( 40.27526882409969033, 122.9297705074272926, 30.44471234641811819 ) ) ;
#16016 = EDGE_CURVE ( 'NONE', #9530, #20615, #15880, .T. ) ;
#16017 = CARTESIAN_POINT ( 'NONE',  ( 44.55648932407425633, 144.6844580088725820, 38.96596240072933170 ) ) ;
#16018 = CARTESIAN_POINT ( 'NONE',  ( 38.01140435219952707, 99.86049967264871441, 35.83527830041809636 ) ) ;
#16019 = CARTESIAN_POINT ( 'NONE',  ( 38.01140435219952707, 129.7104996726487514, 34.21067981925357060 ) ) ;
#16020 = CARTESIAN_POINT ( 'NONE',  ( -157.6495955161842062, -176.9391397928654612, 41.15050349809589392 ) ) ;
#16021 = CARTESIAN_POINT ( 'NONE',  ( -157.6495955161842062, -194.0391397928654271, 58.16351966513671812 ) ) ;
#16022 = CARTESIAN_POINT ( 'NONE',  ( 48.01140435219951996, 74.06049967264874567, 35.83527830041809636 ) ) ;
#16023 = CARTESIAN_POINT ( 'NONE',  ( -151.4692556286852891, -186.2391397928655010, 39.65701158161630246 ) ) ;
#16024 = CARTESIAN_POINT ( 'NONE',  ( -161.4692556286852607, -160.7130981290892748, 46.40781461928724383 ) ) ;
#16025 = CARTESIAN_POINT ( 'NONE',  ( 38.01140435219952707, 128.7844580088725763, 34.21067981925357060 ) ) ;
#16026 = CARTESIAN_POINT ( 'NONE',  ( 47.43856463449117200, 104.0297705074273011, 32.77220824515698183 ) ) ;
#16027 = CARTESIAN_POINT ( 'NONE',  ( 43.42882498487155374, 148.1844126167958393, 2.937742163556189112 ) ) ;
#16028 = DIRECTION ( 'NONE',  ( 0.000000000000000000, 1.000000000000000000, 0.000000000000000000 ) ) ;
#16029 = CARTESIAN_POINT ( 'NONE',  ( 46.59305225739526435, 100.9151871740940010, 31.60846029578754468 ) ) ;
#16030 = CARTESIAN_POINT ( 'NONE',  ( 43.01140435219951286, 134.9604996726487514, 29.21067981925356705 ) ) ;
#16031 = EDGE_LOOP ( 'NONE', ( #11248, #278, #12912, #6867 ) ) ;
#16032 = CARTESIAN_POINT ( 'NONE',  ( 48.01140435219951996, 76.13445800887258486, 35.83527830041809636 ) ) ;
#16033 = CARTESIAN_POINT ( 'NONE',  ( 13.78455932396994577, 137.7305411390292420, 2.696406107442721467 ) ) ;
#16034 = CARTESIAN_POINT ( 'NONE',  ( 40.94005093944240059, 91.86375568685591020, -12.50564155961141566 ) ) ;
#16035 = CARTESIAN_POINT ( 'NONE',  ( 23.17700876947760591, 147.8092992330439586, -3.851376987104358829 ) ) ;
#16036 = AXIS2_PLACEMENT_3D ( 'NONE', #6365, #19931, #2946 ) ;
#16037 = CARTESIAN_POINT ( 'NONE',  ( 46.59305225739526435, 79.57977050742731251, 36.81289934271958941 ) ) ;
#16038 = AXIS2_PLACEMENT_3D ( 'NONE', #8111, #14817, #18245 ) ;
#16039 = ORIENTED_EDGE ( 'NONE', *, *, #11740, .F. ) ;
#16040 = ORIENTED_EDGE ( 'NONE', *, *, #16699, .T. ) ;
#16041 = FACE_OUTER_BOUND ( 'NONE', #18158, .T. ) ;
#16042 = AXIS2_PLACEMENT_3D ( 'NONE', #6077, #11147, #4642 ) ;
#16043 = PLANE ( 'NONE',  #4192 ) ;
#16044 = AXIS2_PLACEMENT_3D ( 'NONE', #1680, #11592, #8079 ) ;
#16046 = ADVANCED_FACE ( 'NONE', ( #3059 ), #7814, .T. ) ;
#16045 = CARTESIAN_POINT ( 'NONE',  ( 38.01140435219951996, 123.5604996726487315, 32.58608133808903773 ) ) ;
#16048 = CARTESIAN_POINT ( 'NONE',  ( 60.78979090282389564, 90.74622564588611340, -6.275468401765792237 ) ) ;
#16047 = CARTESIAN_POINT ( 'NONE',  ( 47.43856463449118621, 73.61518717409400381, 34.21067981925357060 ) ) ;
#16049 = EDGE_CURVE ( 'NONE', #735, #18451, #17927, .T. ) ;
#16050 = CARTESIAN_POINT ( 'NONE',  ( -148.5561028927606344, -168.9938272943107336, 58.62277379824867296 ) ) ;
#16051 = CARTESIAN_POINT ( 'NONE',  ( 44.55648932407425633, 112.6104996726487428, 38.96596240072933170 ) ) ;
#16052 = CARTESIAN_POINT ( 'NONE',  ( -141.4692556286852891, -185.9130981290892919, 46.40781461928724383 ) ) ;
#16053 = PLANE ( 'NONE',  #13886 ) ;
#16054 = CARTESIAN_POINT ( 'NONE',  ( 38.01140435219952707, 149.9344580088725820, 35.83527830041809636 ) ) ;
#16055 = CARTESIAN_POINT ( 'NONE',  ( 38.58424406990784661, 144.2297705074273324, 32.77220824515698183 ) ) ;
#16056 = ADVANCED_FACE ( 'NONE', ( #3693 ), #14841, .F. ) ;
#16057 = CARTESIAN_POINT ( 'NONE',  ( 76.86499250339331013, 125.5074929390188316, 4.406300711698651895 ) ) ;
#16058 = CARTESIAN_POINT ( 'NONE',  ( 45.74753988029934249, 122.0651871740940209, 30.44471234641812174 ) ) ;
#16059 = CARTESIAN_POINT ( 'NONE',  ( -151.4692556286853176, -174.8130981290893260, 59.65701158161632378 ) ) ;
#16060 = CARTESIAN_POINT ( 'NONE',  ( 43.01140435219951286, 122.0344580088725763, 29.21067981925356705 ) ) ;
#16061 = DIRECTION ( 'NONE',  ( 1.000000000000000000, 0.000000000000000000, 0.000000000000000000 ) ) ;
#16062 = AXIS2_PLACEMENT_3D ( 'NONE', #21321, #21431, #11385 ) ;
#16063 = CARTESIAN_POINT ( 'NONE',  ( 43.01140435219951996, 119.9070776186055838, -19.99999999999997868 ) ) ;
#16064 = CARTESIAN_POINT ( 'NONE',  ( 48.57925227495098852, 92.17995633088730756, 20.19957357060707182 ) ) ;
#16065 = FACE_OUTER_BOUND ( 'NONE', #10500, .T. ) ;
#16066 = CARTESIAN_POINT ( 'NONE',  ( 46.59305225739526435, 106.9151871740940152, 31.60846029578754468 ) ) ;
#16067 = ORIENTED_EDGE ( 'NONE', *, *, #21520, .T. ) ;
#16068 = CARTESIAN_POINT ( 'NONE',  ( -149.8854112254399240, -157.6622583705452030, 59.65701158161632378 ) ) ;
#16069 = EDGE_LOOP ( 'NONE', ( #19128, #15696 ) ) ;
#16070 = CARTESIAN_POINT ( 'NONE',  ( 39.92123440845004723, 95.33445800887255928, 29.95742577749337343 ) ) ;
#16071 = DIRECTION ( 'NONE',  ( 1.000000000000000000, 0.000000000000000000, 0.000000000000000000 ) ) ;
#16072 = VECTOR ( 'NONE', #15087, 1000.000000000000000 ) ;
#16073 = PRODUCT_DEFINITION_SHAPE ( 'NONE', 'NONE',  #21832 ) ;
#16074 = CARTESIAN_POINT ( 'NONE',  ( 41.46631938032478359, 148.3104996726487457, 38.96596240072933170 ) ) ;
#16076 = CARTESIAN_POINT ( 'NONE',  ( 50.40261314387542768, 147.0381507142914188, -1.791644202716362821 ) ) ;
#16075 = CARTESIAN_POINT ( 'NONE',  ( 45.74753988029933538, 109.1651871740939868, 37.97664729208901946 ) ) ;
#16077 =( BOUNDED_CURVE ( )  B_SPLINE_CURVE ( 2, ( #19810, #1290, #11417, #6468, #21690, #11204, #4476, #16377, #10005, #16709, #15061, #11642, #3273 ),
 .UNSPECIFIED., .F., .F. ) 
 B_SPLINE_CURVE_WITH_KNOTS ( ( 3, 2, 2, 2, 2, 2, 3 ),
 ( 0.02205882352941176960, 0.02352941176470588203, 0.02647058823529411728, 0.02941176470588235253, 0.03235294117647059126, 0.03529411764705882304, 0.03676470588235293546 ),
 .UNSPECIFIED. ) 
 CURVE ( )  GEOMETRIC_REPRESENTATION_ITEM ( )  RATIONAL_B_SPLINE_CURVE ( ( 0.9755282581475767101, 0.9755282581475768211, 1.000000000000000000, 0.9510565162951535312, 1.000000000000000000, 0.9510565162951535312, 1.000000000000000000, 0.9510565162951535312, 1.000000000000000000, 0.9510565162951535312, 1.000000000000000000, 0.9755282581475768211, 0.9755282581475767101 ) ) 
 REPRESENTATION_ITEM ( '' )  );
#16078 = CARTESIAN_POINT ( 'NONE',  ( 39.92123440845004723, 67.16049967264873999, 38.46393386101376421 ) ) ;
#16080 = CARTESIAN_POINT ( 'NONE',  ( 43.01140435219951286, 60.53445800887258343, 39.21067981925356349 ) ) ;
#16079 = CARTESIAN_POINT ( 'NONE',  ( -9.888205435155610346, 14.72870593739803624, -19.99999999999997868 ) ) ;
#16081 = CARTESIAN_POINT ( 'NONE',  ( 43.80332655382220253, 117.6113394311928317, 39.21067981925355639 ) ) ;
#16082 = CARTESIAN_POINT ( 'NONE',  ( 43.80332655382220253, 78.61133943119283174, 39.21067981925355639 ) ) ;
#16083 = DIRECTION ( 'NONE',  ( 0.000000000000000000, 1.000000000000000000, 0.000000000000000000 ) ) ;
#16084 = CARTESIAN_POINT ( 'NONE',  ( 47.43856463449118621, 73.61518717409400381, 34.21067981925357060 ) ) ;
#16085 = EDGE_CURVE ( 'NONE', #19572, #6509, #15484, .T. ) ;
#16086 = CARTESIAN_POINT ( 'NONE',  ( 10.42839491720816625, 130.4056617841633283, -4.565575592310756825 ) ) ;
#16087 = AXIS2_PLACEMENT_3D ( 'NONE', #11851, #3486, #1826 ) ;
#16088 = CARTESIAN_POINT ( 'NONE',  ( 38.01140435219952707, 114.5604996726487315, 32.58608133808903773 ) ) ;
#16089 = CARTESIAN_POINT ( 'NONE',  ( -145.6429501568359797, -174.8438272943107279, 57.67623309621198047 ) ) ;
#16090 = CARTESIAN_POINT ( 'NONE',  ( -151.4692556286852891, -181.4084106276440025, 59.56931450028537256 ) ) ;
#16091 = ORIENTED_EDGE ( 'NONE', *, *, #11935, .F. ) ;
#16092 = CARTESIAN_POINT ( 'NONE',  ( -142.0420953463936087, -171.6584106276440593, 49.65701158161630957 ) ) ;
#16093 = CARTESIAN_POINT ( 'NONE',  ( 63.99609067623438108, 147.0574274800572425, 3.572798616028722396 ) ) ;
#16094 = AXIS2_PLACEMENT_3D ( 'NONE', #8483, #1854, #21814 ) ;
#16095 = ORIENTED_EDGE ( 'NONE', *, *, #12715, .T. ) ;
#16096 = CARTESIAN_POINT ( 'NONE',  ( 47.43856463449118621, 133.6151871740940180, 34.21067981925357060 ) ) ;
#16097 = CARTESIAN_POINT ( 'NONE',  ( 41.64333658814960870, 92.77977050742731535, 30.00020018409699318 ) ) ;
#16098 = ORIENTED_EDGE ( 'NONE', *, *, #10327, .F. ) ;
#16099 = VERTEX_POINT ( 'NONE', #8769 ) ;
#16100 = CARTESIAN_POINT ( 'NONE',  ( 63.85057544308668298, 100.9084186779620609, 13.48995955233852229 ) ) ;
#16101 = ORIENTED_EDGE ( 'NONE', *, *, #1239, .T. ) ;
#16102 = CARTESIAN_POINT ( 'NONE',  ( 39.92123440845004723, 116.3344580088725735, 29.95742577749337343 ) ) ;
#16103 = AXIS2_PLACEMENT_3D ( 'NONE', #11517, #13068, #14602 ) ;
#16104 = CARTESIAN_POINT ( 'NONE',  ( 33.01140435219951286, 119.9070776186055838, -19.99999999999997868 ) ) ;
#16105 = EDGE_CURVE ( 'NONE', #13613, #4745, #3598, .T. ) ;
#16106 = ADVANCED_FACE ( 'NONE', ( #18269 ), #20559, .T. ) ;
#16107 = VECTOR ( 'NONE', #13066, 1000.000000000000000 ) ;
#16108 = CARTESIAN_POINT ( 'NONE',  ( 45.74753988029933538, 80.32977050742731251, 30.44471234641811819 ) ) ;
#16109 = CARTESIAN_POINT ( 'NONE',  ( 46.59305225739526435, 133.9151871740940010, 31.60846029578754468 ) ) ;
#16110 = CIRCLE ( 'NONE', #15724, 13.99821153497579651 ) ;
#16111 = CARTESIAN_POINT ( 'NONE',  ( 41.46631938032478359, 96.11049967264874283, 29.45539723777780239 ) ) ;
#16112 = COLOUR_RGB ( '', 0.09019608, 0.27058824, 0.51372549) ;
#16113 = CARTESIAN_POINT ( 'NONE',  ( 55.94180145820917716, 151.6039095241057453, 11.26783467880839140 ) ) ;
#16114 = FACE_OUTER_BOUND ( 'NONE', #5740, .T. ) ;
#16115 = CARTESIAN_POINT ( 'NONE',  ( -161.4692556286852607, -161.6391397928654783, 46.40781461928724383 ) ) ;
#16116 = CARTESIAN_POINT ( 'NONE',  ( -141.4692556286852891, -159.0630981290892976, 49.65701158161630957 ) ) ;
#16117 = CARTESIAN_POINT ( 'NONE',  ( 46.10157429594899270, 106.7604996726487201, 38.46393386101375711 ) ) ;
#16118 = CARTESIAN_POINT ( 'NONE',  ( -153.0531000319306258, -184.8160212151856854, 59.65701158161632378 ) ) ;
#16119 = EDGE_LOOP ( 'NONE', ( #11654, #14528, #15699, #9260 ) ) ;
#16120 = CARTESIAN_POINT ( 'NONE',  ( 38.58424406990786082, 72.37977050742732388, 34.21067981925357060 ) ) ;
#16121 = CARTESIAN_POINT ( 'NONE',  ( -143.8425227516148084, -159.6938272943107222, 55.19815736654470584 ) ) ;
#16122 = CARTESIAN_POINT ( 'NONE',  ( 8.944919112598912037, 123.2842988173194385, -4.803623532975393573 ) ) ;
#16123 = CARTESIAN_POINT ( 'NONE',  ( 2.004595370269653287, 635.3380690778678854, -0.8325491102011938205 ) ) ;
#16124 = ORIENTED_EDGE ( 'NONE', *, *, #11768, .F. ) ;
#16125 = LINE ( 'NONE', #16228, #7621 ) ;
#16126 = CARTESIAN_POINT ( 'NONE',  ( 39.92123440845005433, 105.2344580088725650, 38.46393386101375711 ) ) ;
#16127 = CARTESIAN_POINT ( 'NONE',  ( 47.43856463449117911, 127.7297705074272898, 35.64915139335015937 ) ) ;
#16128 = ORIENTED_EDGE ( 'NONE', *, *, #11356, .T. ) ;
#16129 = ORIENTED_EDGE ( 'NONE', *, *, #8212, .F. ) ;
#16130 = CARTESIAN_POINT ( 'NONE',  ( 38.58424406990784661, 129.5297705074273154, 35.64915139335016647 ) ) ;
#16131 = FACE_OUTER_BOUND ( 'NONE', #1245, .T. ) ;
#16132 = EDGE_CURVE ( 'NONE', #2768, #6540, #17227, .T. ) ;
#16133 = CARTESIAN_POINT ( 'NONE',  ( 48.01140435219951996, 64.28445800887257633, 34.21067981925357060 ) ) ;
#16134 = CARTESIAN_POINT ( 'NONE',  ( -9.888205435155610346, 14.72870593739803624, -35.00000000000000000 ) ) ;
#16135 = CARTESIAN_POINT ( 'NONE',  ( 83.67254549292280785, -61.68114226949890622, 20.00000000000000355 ) ) ;
#16136 = CARTESIAN_POINT ( 'NONE',  ( 38.01140435219952707, 96.86049967264871441, 35.83527830041809636 ) ) ;
#16137 = CARTESIAN_POINT ( 'NONE',  ( -151.4692556286852891, -186.2391397928654726, 39.14238933923362396 ) ) ;
#16138 = CARTESIAN_POINT ( 'NONE',  ( 47.05648932407426344, 74.51049967264873430, 31.27175355779120025 ) ) ;
#16139 = LINE ( 'NONE', #19342, #11433 ) ;
#16140 = CARTESIAN_POINT ( 'NONE',  ( -142.0420953463936087, -192.3938272943107393, 49.65701158161630957 ) ) ;
#16141 = CARTESIAN_POINT ( 'NONE',  ( 41.46631938032478359, 137.1844580088725820, 29.45539723777780239 ) ) ;
#16142 = CARTESIAN_POINT ( 'NONE',  ( 47.43856463449118621, 103.8797705074273239, 34.21067981925357060 ) ) ;
#16143 =( BOUNDED_CURVE ( )  B_SPLINE_CURVE ( 2, ( #11230, #9377, #2751, #14213, #14538, #19726, #21166, #21279, #11339, #16299, #993, #16082, #1207 ),
 .UNSPECIFIED., .F., .F. ) 
 B_SPLINE_CURVE_WITH_KNOTS ( ( 3, 2, 2, 2, 2, 2, 3 ),
 ( 0.7720588235294117974, 0.7735294117647059098, 0.7764705882352941346, 0.7794117647058823595, 0.7823529411764705843, 0.7852941176470588092, 0.7867647058823529216 ),
 .UNSPECIFIED. ) 
 CURVE ( )  GEOMETRIC_REPRESENTATION_ITEM ( )  RATIONAL_B_SPLINE_CURVE ( ( 0.9755282581475768211, 0.9755282581475768211, 1.000000000000000000, 0.9510565162951535312, 1.000000000000000000, 0.9510565162951535312, 1.000000000000000000, 0.9510565162951535312, 1.000000000000000000, 0.9510565162951535312, 1.000000000000000000, 0.9755282581475768211, 0.9755282581475768211 ) ) 
 REPRESENTATION_ITEM ( '' )  );
#16144 = CARTESIAN_POINT ( 'NONE',  ( 52.31916092102454741, 146.6125112339981627, 3.294994845742023948 ) ) ;
#16145 = CYLINDRICAL_SURFACE ( 'NONE', #9583, 4.999999999999997335 ) ;
#16146 = CARTESIAN_POINT ( 'NONE',  ( 41.64333658814960870, 98.51518717409399528, 30.00020018409699318 ) ) ;
#16147 = DIRECTION ( 'NONE',  ( -0.000000000000000000, -0.000000000000000000, -1.000000000000000000 ) ) ;
#16148 = ORIENTED_EDGE ( 'NONE', *, *, #1662, .T. ) ;
#16149 = LINE ( 'NONE', #17795, #10129 ) ;
#16150 = CARTESIAN_POINT ( 'NONE',  ( 57.94507594753278568, 150.7106492751291569, -2.660852849641732298 ) ) ;
#16151 = CARTESIAN_POINT ( 'NONE',  ( 34.95631105476920197, 146.8486248254830855, -9.410786671241964996 ) ) ;
#16152 = CARTESIAN_POINT ( 'NONE',  ( 43.80529445460960858, 154.1304981347762748, -3.137004163733609907 ) ) ;
#16153 = CARTESIAN_POINT ( 'NONE',  ( 47.43856463449117911, 64.72977050742731819, 35.64915139335015937 ) ) ;
#16154 = ORIENTED_EDGE ( 'NONE', *, *, #5437, .F. ) ;
#16155 = ORIENTED_EDGE ( 'NONE', *, *, #6177, .T. ) ;
#16156 = VECTOR ( 'NONE', #13432, 1000.000000000000000 ) ;
#16157 = DIRECTION ( 'NONE',  ( 0.000000000000000000, -1.000000000000000000, 0.000000000000000000 ) ) ;
#16158 = CARTESIAN_POINT ( 'NONE',  ( 41.46631938032478359, 120.1104996726487570, 29.45539723777780239 ) ) ;
#16160 = CARTESIAN_POINT ( 'NONE',  ( 9.997522862669264043, 111.1595821513141402, 9.795857695845493041 ) ) ;
#16159 = CARTESIAN_POINT ( 'NONE',  ( 41.64333658814960870, 74.51518717409399528, 30.00020018409699318 ) ) ;
#16161 = DIRECTION ( 'NONE',  ( 1.000000000000000000, 0.000000000000000000, 0.000000000000000000 ) ) ;
#16162 = CARTESIAN_POINT ( 'NONE',  ( -145.6429501568359797, -168.8438272943107563, 57.67623309621197336 ) ) ;
#16163 = CARTESIAN_POINT ( 'NONE',  ( 62.34613790317991544, 148.1570561279473850, 11.50573666851796339 ) ) ;
#16164 = CARTESIAN_POINT ( 'NONE',  ( -151.4692556286852891, -189.8130981290892692, 60.17163382399899518 ) ) ;
#16165 = CARTESIAN_POINT ( 'NONE',  ( 148.6725454929228079, -61.68114226949890622, -46.21320343559645494 ) ) ;
#16166 = CARTESIAN_POINT ( 'NONE',  ( 43.01140435219951996, 10.71049967264875491, 29.21067981925357060 ) ) ;
#16167 = CARTESIAN_POINT ( 'NONE',  ( 47.43856463449117200, 131.0297705074272869, 32.77220824515698183 ) ) ;
#16168 = CARTESIAN_POINT ( 'NONE',  ( 11.58389279593228238, 133.6817500236834917, 1.549157854527217104 ) ) ;
#16169 = CARTESIAN_POINT ( 'NONE',  ( 38.58424406990785371, 125.9651871740939697, 32.77220824515697473 ) ) ;
#16170 = CARTESIAN_POINT ( 'NONE',  ( 147.5268905834513475, 193.0332408774651185, -5.999999999999950262 ) ) ;
#16171 = CARTESIAN_POINT ( 'NONE',  ( 43.01140435219951996, 10.71049967264875491, 34.21067981925357060 ) ) ;
#16172 = APPLICATION_CONTEXT ( 'automotive_design' ) ;
#16173 = FACE_BOUND ( 'NONE', #4765, .T. ) ;
#16174 = CARTESIAN_POINT ( 'NONE',  ( 43.01140435219951996, 10.71049967264875491, 39.21067981925356349 ) ) ;
#16175 = CARTESIAN_POINT ( 'NONE',  ( 57.39747520560054284, 144.1616143014069280, -9.486357586414486676 ) ) ;
#16176 = CARTESIAN_POINT ( 'NONE',  ( -148.3790856849358306, -186.3891397928654783, 40.14644641866477315 ) ) ;
#16177 = CARTESIAN_POINT ( 'NONE',  ( 44.37947211624943833, 107.2151871740940123, 30.00020018409699318 ) ) ;
#16178 = ORIENTED_EDGE ( 'NONE', *, *, #5263, .F. ) ;
#16179 = DIRECTION ( 'NONE',  ( 0.000000000000000000, 0.000000000000000000, 1.000000000000000000 ) ) ;
#16180 = ORIENTED_EDGE ( 'NONE', *, *, #14765, .T. ) ;
#16181 = CARTESIAN_POINT ( 'NONE',  ( 38.01140435219951996, 95.63445800887255643, 32.58608133808903773 ) ) ;
#16182 = CARTESIAN_POINT ( 'NONE',  ( 43.01140435219951286, 84.53445800887256212, 39.21067981925356349 ) ) ;
#16183 = CARTESIAN_POINT ( 'NONE',  ( 48.01140435219951996, 146.2104996726487229, 34.21067981925357060 ) ) ;
#16185 = CARTESIAN_POINT ( 'NONE',  ( 17.40773937504753377, 131.5336607133424991, -10.36307277412196903 ) ) ;
#16184 = CARTESIAN_POINT ( 'NONE',  ( 41.64333658814960870, 110.5151871740940095, 30.00020018409699318 ) ) ;
#16186 = CARTESIAN_POINT ( 'NONE',  ( 45.51148226160370314, 59.71123016864974176, 29.88059778228138086 ) ) ;
#16188 = CARTESIAN_POINT ( 'NONE',  ( 43.01140435219951996, 147.5344580088726048, 39.21067981925356349 ) ) ;
#16187 = DIRECTION ( 'NONE',  ( 0.000000000000000000, 0.000000000000000000, 1.000000000000000000 ) ) ;
#16189 = SURFACE_STYLE_FILL_AREA ( #2635 ) ;
#16190 = CARTESIAN_POINT ( 'NONE',  ( -38.21168032741934439, -23.19216891395253910, 4.000000000000021316 ) ) ;
#16191 = DIRECTION ( 'NONE',  ( -0.000000000000000000, -0.000000000000000000, -1.000000000000000000 ) ) ;
#16192 = CARTESIAN_POINT ( 'NONE',  ( 41.64333658814960870, 65.51518717409400949, 30.00020018409699318 ) ) ;
#16193 = CARTESIAN_POINT ( 'NONE',  ( 55.11952973528949684, 87.88698225678692211, -7.065691903092018222 ) ) ;
#16194 = CARTESIAN_POINT ( 'NONE',  ( 44.55648932407425633, 94.61049967264874283, 38.96596240072933170 ) ) ;
#16195 = CARTESIAN_POINT ( 'NONE',  ( -145.6429501568359797, -173.9438272943106938, 41.63779006702063867 ) ) ;
#16196 = CARTESIAN_POINT ( 'NONE',  ( -143.8425227516148084, -186.3584106276440480, 44.11586579668791330 ) ) ;
#16197 = ORIENTED_EDGE ( 'NONE', *, *, #20907, .T. ) ;
#16198 = CARTESIAN_POINT ( 'NONE',  ( 38.58424406990785371, 65.96518717409398391, 32.77220824515697473 ) ) ;
#16199 = CARTESIAN_POINT ( 'NONE',  ( -160.8964159109769696, -170.1584106276440593, 49.65701158161630957 ) ) ;
#16200 = CARTESIAN_POINT ( 'NONE',  ( 43.13803657676253067, 85.59359249887060628, 13.33475322466254198 ) ) ;
#16201 = DIRECTION ( 'NONE',  ( 0.000000000000000000, 1.000000000000000000, 0.000000000000000000 ) ) ;
#16202 = CARTESIAN_POINT ( 'NONE',  ( 41.64333658814960870, 131.5151871740939953, 30.00020018409699318 ) ) ;
#16203 = AXIS2_PLACEMENT_3D ( 'NONE', #2300, #20613, #10691 ) ;
#16204 = ORIENTED_EDGE ( 'NONE', *, *, #3400, .F. ) ;
#16205 = VERTEX_POINT ( 'NONE', #11542 ) ;
#16206 = EDGE_CURVE ( 'NONE', #21208, #4150, #4751, .T. ) ;
#16207 = PRESENTATION_STYLE_ASSIGNMENT (( #9510 ) ) ;
#16208 = EDGE_LOOP ( 'NONE', ( #2877, #8016, #5319, #12613, #17932, #8558, #21243, #11985, #5112, #20905, #14799, #8207, #13240, #20137, #11855, #9061, #19327, #4772, #8070, #5270, #16862, #1558, #11716, #11383, #7880, #12356, #4114, #14459, #17312, #14143, #15129, #806, #18766, #20165, #15796, #18423, #21790, #21762, #13684, #6749, #11463, #7790, #3880, #13101, #18048, #17417, #18635, #17902, #11579, #21597, #17633, #5110, #11581, #14030, #1475, #16529, #3992, #13204, #13637, #20990, #20060, #10881, #1986, #8771, #1556, #3493, #14851, #6234, #20582, #3539, #1448 ) ) ;
#16209 =( BOUNDED_CURVE ( )  B_SPLINE_CURVE ( 2, ( #9981, #16246, #21553, #9869, #3252, #11506, #14918, #6218, #1155, #6444, #11180, #14591, #14482 ),
 .UNSPECIFIED., .F., .F. ) 
 B_SPLINE_CURVE_WITH_KNOTS ( ( 3, 2, 2, 2, 2, 2, 3 ),
 ( 0.2720588235294117974, 0.2735294117647059098, 0.2764705882352941346, 0.2794117647058823595, 0.2823529411764705843, 0.2852941176470588092, 0.2867647058823529216 ),
 .UNSPECIFIED. ) 
 CURVE ( )  GEOMETRIC_REPRESENTATION_ITEM ( )  RATIONAL_B_SPLINE_CURVE ( ( 0.9755282581475768211, 0.9755282581475772652, 1.000000000000000000, 0.9510565162951535312, 1.000000000000000000, 0.9510565162951535312, 1.000000000000000000, 0.9510565162951535312, 1.000000000000000000, 0.9510565162951535312, 1.000000000000000000, 0.9755282581475768211, 0.9755282581475768211 ) ) 
 REPRESENTATION_ITEM ( '' )  );
#16210 = ADVANCED_FACE ( 'NONE', ( #9902 ), #20449, .T. ) ;
#16211 = CARTESIAN_POINT ( 'NONE',  ( 41.46631938032478359, 116.1844580088725820, 29.45539723777780239 ) ) ;
#16212 = CARTESIAN_POINT ( 'NONE',  ( 45.05633291560663167, 59.76197383743924973, 29.61780626570246966 ) ) ;
#16213 = CARTESIAN_POINT ( 'NONE',  ( 38.58424406990786082, 78.37977050742732388, 34.21067981925357060 ) ) ;
#16214 = CARTESIAN_POINT ( 'NONE',  ( 40.27526882409969033, 137.6651871740940294, 30.44471234641811819 ) ) ;
#16215 = ADVANCED_FACE ( 'NONE', ( #15583 ), #18685, .F. ) ;
#16216 = CARTESIAN_POINT ( 'NONE',  ( 47.05648932407426344, 94.91049967264873999, 37.14960608071593384 ) ) ;
#16217 = CARTESIAN_POINT ( 'NONE',  ( 38.54497605562327323, 85.96704844161884296, 14.48200433579215662 ) ) ;
#16218 = LINE ( 'NONE', #7863, #2952 ) ;
#16219 = CARTESIAN_POINT ( 'NONE',  ( -145.2889157411863721, -157.4391397928654612, 58.16351966513671812 ) ) ;
#16220 = CARTESIAN_POINT ( 'NONE',  ( 173.3794444120442506, -84.13255853780189852, 5.000000000000018652 ) ) ;
#16221 = DIRECTION ( 'NONE',  ( 0.000000000000000000, 1.000000000000000000, 0.000000000000000000 ) ) ;
#16222 = ORIENTED_EDGE ( 'NONE', *, *, #21681, .T. ) ;
#16223 = CARTESIAN_POINT ( 'NONE',  ( 46.59305225739526435, 71.17977050742730682, 31.60846029578754468 ) ) ;
#16224 = CARTESIAN_POINT ( 'NONE',  ( -148.5561028927606344, -195.0584106276440650, 40.69124936498395328 ) ) ;
#16225 = CARTESIAN_POINT ( 'NONE',  ( 51.78234217841457365, 152.9971814535558963, 4.124977536042813142 ) ) ;
#16226 = CARTESIAN_POINT ( 'NONE',  ( -157.2955611005346270, -188.6084106276440764, 41.63779006702063867 ) ) ;
#16227 = ORIENTED_EDGE ( 'NONE', *, *, #12414, .T. ) ;
#16228 = CARTESIAN_POINT ( 'NONE',  ( 93.25569916848381524, 126.0916958004080755, 272.0939500981630204 ) ) ;
#16229 = CARTESIAN_POINT ( 'NONE',  ( -56.84366818088135176, 789.5005544000622422, -19.99999999999997868 ) ) ;
#16230 = CARTESIAN_POINT ( 'NONE',  ( 47.43856463449117911, 125.0297705074273011, 32.77220824515697473 ) ) ;
#16231 = VERTEX_POINT ( 'NONE', #12161 ) ;
#16232 = EDGE_CURVE ( 'NONE', #5984, #7609, #12058, .T. ) ;
#16233 = CARTESIAN_POINT ( 'NONE',  ( 43.01140435219951286, 87.53445800887257633, 39.21067981925356349 ) ) ;
#16234 = VERTEX_POINT ( 'NONE', #1520 ) ;
#16235 = CARTESIAN_POINT ( 'NONE',  ( 41.64333658814960870, 128.7797705074273438, 30.00020018409699318 ) ) ;
#16236 = DIRECTION ( 'NONE',  ( 0.9385982292947088190, 0.3450121214752274179, -1.836742322155470491E-16 ) ) ;
#16237 = CARTESIAN_POINT ( 'NONE',  ( 38.58424406990784661, 90.52977050742731535, 35.64915139335016647 ) ) ;
#16238 = CARTESIAN_POINT ( 'NONE',  ( 38.01140435219951996, 65.63445800887257064, 32.58608133808903773 ) ) ;
#16239 = AXIS2_PLACEMENT_3D ( 'NONE', #3453, #240, #17092 ) ;
#16240 = AXIS2_PLACEMENT_3D ( 'NONE', #8535, #2226, #5636 ) ;
#16241 = CARTESIAN_POINT ( 'NONE',  ( 72.34521997529867576, 314.8592298662555322, 272.0939500981630204 ) ) ;
#16242 = CARTESIAN_POINT ( 'NONE',  ( 38.01140435219952707, 101.6344580088725849, 32.58608133808903773 ) ) ;
#16243 = CARTESIAN_POINT ( 'NONE',  ( -161.4692556286853176, -176.4891397928654442, 49.65701158161630957 ) ) ;
#16244 = CARTESIAN_POINT ( 'NONE',  ( -154.5594255724347761, -184.8891397928654783, 59.16757674456785310 ) ) ;
#16245 = CARTESIAN_POINT ( 'NONE',  ( 38.96631938032478359, 89.48445800887257917, 31.27175355779120025 ) ) ;
#16246 = CARTESIAN_POINT ( 'NONE',  ( 43.80332655382221674, 131.8836182503284533, 29.21067981925357060 ) ) ;
#16247 = CARTESIAN_POINT ( 'NONE',  ( -159.0959885057557983, -190.5938272943107279, 55.19815736654470584 ) ) ;
#16248 = APPLICATION_PROTOCOL_DEFINITION ( 'draft international standard', 'automotive_design', 1998, #6034 ) ;
#16249 = AXIS2_PLACEMENT_3D ( 'NONE', #1942, #3271, #21796 ) ;
#16250 = CARTESIAN_POINT ( 'NONE',  ( 44.55648932407425633, 121.8844580088725849, 29.45539723777780239 ) ) ;
#16251 = CARTESIAN_POINT ( 'NONE',  ( 40.27526882409969033, 101.9297705074273068, 30.44471234641811819 ) ) ;
#16252 = CARTESIAN_POINT ( 'NONE',  ( 68.93731127356984700, 108.6095829621005180, 19.12825547442421126 ) ) ;
#16253 = CARTESIAN_POINT ( 'NONE',  ( -157.2955611005346270, -187.4438272943106938, 57.67623309621198047 ) ) ;
#16254 = CARTESIAN_POINT ( 'NONE',  ( 39.42975644700377558, 96.41518717409400097, 36.81289934271958941 ) ) ;
#16255 = DIRECTION ( 'NONE',  ( 0.3450121214752278065, -0.9385982292947087080, 0.000000000000000000 ) ) ;
#16256 = ORIENTED_EDGE ( 'NONE', *, *, #21756, .F. ) ;
#16257 = FACE_BOUND ( 'NONE', #6402, .T. ) ;
#16258 = CARTESIAN_POINT ( 'NONE',  ( 76.79083979644461522, 114.3551126354810492, -1.232281421064668869 ) ) ;
#16259 = CARTESIAN_POINT ( 'NONE',  ( 58.12682455153977656, 96.19528378222683784, -13.22021563155647428 ) ) ;
#16260 = PRODUCT_DEFINITION_SHAPE ( 'NONE', 'NONE',  #11071 ) ;
#16261 = AXIS2_PLACEMENT_3D ( 'NONE', #765, #20831, #2096 ) ;
#16262 = AXIS2_PLACEMENT_3D ( 'NONE', #11109, #2734, #12986 ) ;
#16263 = CARTESIAN_POINT ( 'NONE',  ( 47.43856463449117911, 70.72977050742730398, 35.64915139335015937 ) ) ;
#16264 = ORIENTED_EDGE ( 'NONE', *, *, #18272, .T. ) ;
#16265 = ORIENTED_EDGE ( 'NONE', *, *, #6546, .F. ) ;
#16266 = CARTESIAN_POINT ( 'NONE',  ( 38.58424406990784661, 156.2297705074273040, 32.77220824515698183 ) ) ;
#16267 = LINE ( 'NONE', #10989, #8444 ) ;
#16268 = CARTESIAN_POINT ( 'NONE',  ( 46.10157429594899270, 112.7604996726487485, 38.46393386101376421 ) ) ;
#16270 = CARTESIAN_POINT ( 'NONE',  ( 28.88048086162541850, 151.0887240815949895, -10.63664014359656385 ) ) ;
#16269 = CARTESIAN_POINT ( 'NONE',  ( 47.43856463449117200, 64.76518717409400949, 32.77220824515698183 ) ) ;
#16271 = CARTESIAN_POINT ( 'NONE',  ( 41.46631938032478359, 66.38445800887257064, 38.96596240072933170 ) ) ;
#16272 =( BOUNDED_CURVE ( )  B_SPLINE_CURVE ( 2, ( #5997, #4449, #9436, #17784, #12835, #12727, #17463, #19451, #9111, #2692, #2805, #12401, #15708 ),
 .UNSPECIFIED., .F., .F. ) 
 B_SPLINE_CURVE_WITH_KNOTS ( ( 3, 2, 2, 2, 2, 2, 3 ),
 ( 0.9044117647058823595, 0.9058823529411764719, 0.9088235294117646967, 0.9117647058823529216, 0.9147058823529411464, 0.9176470588235293713, 0.9191176470588234837 ),
 .UNSPECIFIED. ) 
 CURVE ( )  GEOMETRIC_REPRESENTATION_ITEM ( )  RATIONAL_B_SPLINE_CURVE ( ( 0.9755282581475768211, 0.9755282581475768211, 1.000000000000000000, 0.9510565162951535312, 1.000000000000000000, 0.9510565162951535312, 1.000000000000000000, 0.9510565162951535312, 1.000000000000000000, 0.9510565162951535312, 1.000000000000000000, 0.9755282581475768211, 0.9755282581475768211 ) ) 
 REPRESENTATION_ITEM ( '' )  );
#16273 = CARTESIAN_POINT ( 'NONE',  ( -159.0959885057557983, -172.5938272943107279, 55.19815736654470584 ) ) ;
#16274 = CARTESIAN_POINT ( 'NONE',  ( 163.3401611601854029, 191.7221236944928364, 21.73429951086134082 ) ) ;
#16275 = CARTESIAN_POINT ( 'NONE',  ( -154.5594255724347761, -176.1630981290893203, 40.14644641866476604 ) ) ;
#16276 = CARTESIAN_POINT ( 'NONE',  ( 134.6380592378699532, 268.5785371414991687, -3.999999999999996447 ) ) ;
#16277 = CARTESIAN_POINT ( 'NONE',  ( 38.96631938032478359, 149.4844580088725934, 31.27175355779120025 ) ) ;
#16278 = CARTESIAN_POINT ( 'NONE',  ( 43.01140435219951286, 136.1297705074273381, 38.86567161673127657 ) ) ;
#16279 = CARTESIAN_POINT ( 'NONE',  ( 71.48324150724619130, 139.0594858779678873, 3.930207297951037848 ) ) ;
#16280 = CARTESIAN_POINT ( 'NONE',  ( 38.58424406990785371, 122.9651871740939981, 32.77220824515697473 ) ) ;
#16281 = EDGE_CURVE ( 'NONE', #14006, #12910, #19932, .T. ) ;
#16282 = CARTESIAN_POINT ( 'NONE',  ( -151.4692556286852891, -157.4084106276440593, 59.56931450028537256 ) ) ;
#16283 = CARTESIAN_POINT ( 'NONE',  ( 43.80332655382218832, 139.5373810949689926, 39.21067981925355639 ) ) ;
#16284 = CARTESIAN_POINT ( 'NONE',  ( 43.01140435219951996, 10.71049967264875491, 59.21067981925356349 ) ) ;
#16285 = CARTESIAN_POINT ( 'NONE',  ( 49.02192908010439254, 147.4586317741252799, -9.843465619175002956 ) ) ;
#16286 = CARTESIAN_POINT ( 'NONE',  ( -149.8854112254399240, -187.6622583705452030, 59.65701158161632378 ) ) ;
#16287 = VERTEX_POINT ( 'NONE', #13713 ) ;
#16288 = ORIENTED_EDGE ( 'NONE', *, *, #9356, .T. ) ;
#16289 = CARTESIAN_POINT ( 'NONE',  ( 44.55648932407425633, 84.68445800887256780, 38.96596240072933170 ) ) ;
#16290 = CYLINDRICAL_SURFACE ( 'NONE', #14745, 4.999999999999997335 ) ;
#16291 = EDGE_CURVE ( 'NONE', #21749, #8531, #19008, .T. ) ;
#16292 = CARTESIAN_POINT ( 'NONE',  ( 44.55648932407425633, 145.6104996726487570, 38.96596240072933170 ) ) ;
#16294 = CARTESIAN_POINT ( 'NONE',  ( 21.63557314705429846, 101.6375443364048152, 2.375099401820868206 ) ) ;
#16293 = CARTESIAN_POINT ( 'NONE',  ( 45.74753988029933538, 101.0651871740939924, 30.44471234641811819 ) ) ;
#16295 = CARTESIAN_POINT ( 'NONE',  ( -142.0420953463936087, -165.6584106276440593, 49.65701158161630957 ) ) ;
#16296 = CARTESIAN_POINT ( 'NONE',  ( 48.01140435219951996, 65.21049967264873715, 34.21067981925357060 ) ) ;
#16298 = FACE_OUTER_BOUND ( 'NONE', #2095, .T. ) ;
#16297 = DIRECTION ( 'NONE',  ( 0.000000000000000000, 0.000000000000000000, 1.000000000000000000 ) ) ;
#16299 = CARTESIAN_POINT ( 'NONE',  ( 46.10157429594899270, 78.83445800887255928, 38.46393386101375711 ) ) ;
#16300 = CARTESIAN_POINT ( 'NONE',  ( -159.5594255724347761, -190.2630981290893146, 55.53486410454104316 ) ) ;
#16301 = CARTESIAN_POINT ( 'NONE',  ( 43.01140435219951286, 60.86518717409400381, 38.86567161673127657 ) ) ;
#16302 = CARTESIAN_POINT ( 'NONE',  ( 43.80529445460960858, 154.1304981347762748, -3.137004163733609907 ) ) ;
#16303 = FACE_OUTER_BOUND ( 'NONE', #11169, .T. ) ;
#16304 = CARTESIAN_POINT ( 'NONE',  ( -143.8425227516148084, -174.0938272943107279, 44.11586579668791330 ) ) ;
#16305 = CARTESIAN_POINT ( 'NONE',  ( -143.8425227516148084, -183.9584106276440707, 55.19815736654470584 ) ) ;
#16306 = ORIENTED_EDGE ( 'NONE', *, *, #9461, .T. ) ;
#16307 = CARTESIAN_POINT ( 'NONE',  ( 43.01140435219951286, 69.86518717409400381, 38.86567161673127657 ) ) ;
#16308 = CARTESIAN_POINT ( 'NONE',  ( -154.3824083646099439, -167.7584106276440536, 40.69124936498395328 ) ) ;
#16309 = CARTESIAN_POINT ( 'NONE',  ( 19.22998607435487273, 95.16999353120945671, 21.19198650444592857 ) ) ;
#16310 = CARTESIAN_POINT ( 'NONE',  ( -97.23064952102208736, 13.78046159333444720, 4.000000000000021316 ) ) ;
#16311 = CARTESIAN_POINT ( 'NONE',  ( 40.27526882409969033, 138.5651871740939498, 37.97664729208901946 ) ) ;
#16312 = EDGE_CURVE ( 'NONE', #40, #8611, #167, .T. ) ;
#16313 = CARTESIAN_POINT ( 'NONE',  ( 20.11427441861009058, 94.56644311770523359, -4.846896973145477183 ) ) ;
#16314 = VERTEX_POINT ( 'NONE', #18790 ) ;
#16315 = ORIENTED_EDGE ( 'NONE', *, *, #20810, .T. ) ;
#16316 = CARTESIAN_POINT ( 'NONE',  ( 23.35610682547305927, 99.68565781958278649, 15.27541961222430444 ) ) ;
#16317 = VERTEX_POINT ( 'NONE', #8137 ) ;
#16318 = CYLINDRICAL_SURFACE ( 'NONE', #7640, 4.999999999999997335 ) ;
#16319 = CARTESIAN_POINT ( 'NONE',  ( 44.37947211624943833, 74.47977050742731819, 30.00020018409699318 ) ) ;
#16321 = CARTESIAN_POINT ( 'NONE',  ( 70.74141321743030630, 114.7826485538520416, 5.870819564965037429 ) ) ;
#16320 = CARTESIAN_POINT ( 'NONE',  ( 45.74753988029933538, 137.0651871740940067, 30.44471234641811819 ) ) ;
#16322 = CARTESIAN_POINT ( 'NONE',  ( 41.46631938032478359, 87.11049967264874283, 29.45539723777780239 ) ) ;
#16323 = CARTESIAN_POINT ( 'NONE',  ( 62.34613790317991544, 148.1570561279473850, 11.50573666851796339 ) ) ;
#16324 = CARTESIAN_POINT ( 'NONE',  ( 39.04181488774997888, 95.22401868161449556, 37.25520735466819389 ) ) ;
#16325 = CARTESIAN_POINT ( 'NONE',  ( -148.3790856849358306, -160.5891397928654953, 59.16757674456786020 ) ) ;
#16326 = CARTESIAN_POINT ( 'NONE',  ( 43.01140435219951286, 92.36518717409398960, 29.55568802177586463 ) ) ;
#16327 = CARTESIAN_POINT ( 'NONE',  ( 47.05648932407426344, 107.5104996726487485, 31.27175355779120025 ) ) ;
#16328 = DIRECTION ( 'NONE',  ( 1.000000000000000000, 0.000000000000000000, 0.000000000000000000 ) ) ;
#16329 = LINE ( 'NONE', #13036, #13793 ) ;
#16330 = ORIENTED_EDGE ( 'NONE', *, *, #10163, .T. ) ;
#16331 = CARTESIAN_POINT ( 'NONE',  ( 47.43856463449118621, 76.87977050742732388, 34.21067981925357060 ) ) ;
#16332 = CARTESIAN_POINT ( 'NONE',  ( -142.0420953463935803, -192.5084106276439968, 46.59394152635518793 ) ) ;
#16333 = EDGE_CURVE ( 'NONE', #497, #4860, #3587, .T. ) ;
#16334 = CARTESIAN_POINT ( 'NONE',  ( 61.01612483116806374, 90.79174121657607088, -0.2798613066081144796 ) ) ;
#16335 = CARTESIAN_POINT ( 'NONE',  ( -151.4692556286852891, -182.9084106276440025, 39.74470866294723947 ) ) ;
#16336 = ORIENTED_EDGE ( 'NONE', *, *, #15069, .F. ) ;
#16337 = CARTESIAN_POINT ( 'NONE',  ( 38.58424406990784661, 158.9651871740940123, 32.77220824515698183 ) ) ;
#16338 = CARTESIAN_POINT ( 'NONE',  ( 147.8787791192428074, -136.9891397928655010, -9.657011581616311346 ) ) ;
#16339 = AXIS2_PLACEMENT_3D ( 'NONE', #1813, #9080, #692 ) ;
#16340 = CARTESIAN_POINT ( 'NONE',  ( 39.42975644700377558, 123.0797705074273267, 31.60846029578754468 ) ) ;
#16341 = ORIENTED_EDGE ( 'NONE', *, *, #16551, .F. ) ;
#16342 = CARTESIAN_POINT ( 'NONE',  ( 43.80332655382221674, 130.9575765865523067, 29.21067981925357060 ) ) ;
#16343 = AXIS2_PLACEMENT_3D ( 'NONE', #8919, #15623, #15524 ) ;
#16344 = ORIENTED_EDGE ( 'NONE', *, *, #13885, .T. ) ;
#16345 = CARTESIAN_POINT ( 'NONE',  ( 40.27526882409969033, 123.8297705074273125, 37.97664729208901946 ) ) ;
#16346 = FACE_OUTER_BOUND ( 'NONE', #3459, .T. ) ;
#16347 = CARTESIAN_POINT ( 'NONE',  ( 39.92123440845004723, 63.23445800887258628, 38.46393386101376421 ) ) ;
#16348 = ADVANCED_FACE ( 'NONE', ( #10741 ), #14595, .T. ) ;
#16349 = DIRECTION ( 'NONE',  ( -0.000000000000000000, -0.000000000000000000, -1.000000000000000000 ) ) ;
#16350 = LINE ( 'NONE', #1044, #18388 ) ;
#16351 = CARTESIAN_POINT ( 'NONE',  ( -154.5594255724347761, -192.0891397928654953, 40.14644641866476604 ) ) ;
#16352 = DIRECTION ( 'NONE',  ( 0.000000000000000000, -1.000000000000000000, 0.000000000000000000 ) ) ;
#16353 = CARTESIAN_POINT ( 'NONE',  ( 38.01140435219952707, 102.8604996726487286, 35.83527830041809636 ) ) ;
#16354 = CARTESIAN_POINT ( 'NONE',  ( -145.6429501568359797, -188.9438272943106938, 41.63779006702063867 ) ) ;
#16355 = CONTEXT_DEPENDENT_SHAPE_REPRESENTATION ( #5216, #6611 ) ;
#16356 = CARTESIAN_POINT ( 'NONE',  ( 39.92123440845004723, 126.2344580088725934, 38.46393386101376421 ) ) ;
#16357 = CARTESIAN_POINT ( 'NONE',  ( 38.58424406990784661, 99.52977050742728693, 35.64915139335016647 ) ) ;
#16358 = CARTESIAN_POINT ( 'NONE',  ( 22.30625593121589390, 139.1551866335812235, 23.00981086756132044 ) ) ;
#16359 = CARTESIAN_POINT ( 'NONE',  ( -145.6429501568359797, -180.8438272943106995, 57.67623309621198047 ) ) ;
#16360 = CARTESIAN_POINT ( 'NONE',  ( 41.64333658814960870, 90.71518717409401233, 38.42115945441014446 ) ) ;
#16361 = CYLINDRICAL_SURFACE ( 'NONE', #9440, 4.999999999999997335 ) ;
#16362 = ORIENTED_EDGE ( 'NONE', *, *, #4258, .F. ) ;
#16363 = CARTESIAN_POINT ( 'NONE',  ( 43.01140435219951286, 128.9604996726487229, 29.21067981925356705 ) ) ;
#16364 = CARTESIAN_POINT ( 'NONE',  ( 40.90832812944997698, 154.0758954209757121, 3.767805038447253452 ) ) ;
#16365 = CARTESIAN_POINT ( 'NONE',  ( 38.58424406990785371, 144.5297705074273154, 35.64915139335015937 ) ) ;
#16366 = CARTESIAN_POINT ( 'NONE',  ( 17.81206540393426252, 132.5069038242342003, 16.68302557436956945 ) ) ;
#16367 = CARTESIAN_POINT ( 'NONE',  ( 47.43856463449117911, 67.72977050742733240, 35.64915139335015937 ) ) ;
#16368 = ORIENTED_EDGE ( 'NONE', *, *, #7326, .T. ) ;
#16369 = ORIENTED_EDGE ( 'NONE', *, *, #5960, .F. ) ;
#16370 = CARTESIAN_POINT ( 'NONE',  ( 47.43856463449117200, 154.7297705074273040, 35.64915139335016647 ) ) ;
#16371 = DIRECTION ( 'NONE',  ( 0.000000000000000000, 0.000000000000000000, 1.000000000000000000 ) ) ;
#16372 = ADVANCED_FACE ( 'NONE', ( #14820 ), #6455, .T. ) ;
#16373 = CARTESIAN_POINT ( 'NONE',  ( 46.10157429594899270, 107.6604996726487116, 29.95742577749337343 ) ) ;
#16374 = CARTESIAN_POINT ( 'NONE',  ( 39.42975644700377558, 69.41518717409400097, 36.81289934271958941 ) ) ;
#16375 = CARTESIAN_POINT ( 'NONE',  ( -39.63192160874126557, -136.9891397928655010, -35.00000000000000000 ) ) ;
#16376 = CARTESIAN_POINT ( 'NONE',  ( -154.3824083646099439, -166.2938272943107165, 58.62277379824867296 ) ) ;
#16377 = CARTESIAN_POINT ( 'NONE',  ( 38.01140435219952707, 155.6344580088725706, 32.58608133808903773 ) ) ;
#16378 = CARTESIAN_POINT ( 'NONE',  ( -159.5594255724347761, -181.2630981290893146, 55.53486410454104316 ) ) ;
#16379 = CYLINDRICAL_SURFACE ( 'NONE', #3691, 10.00000000000000888 ) ;
#16380 = CARTESIAN_POINT ( 'NONE',  ( 47.05648932407426344, 154.5844580088725877, 31.27175355779120025 ) ) ;
#16381 = CARTESIAN_POINT ( 'NONE',  ( 41.64333658814960870, 129.9797705074273040, 38.42115945441014446 ) ) ;
#16382 = CARTESIAN_POINT ( 'NONE',  ( 16.10574266336056226, 141.2029798434031989, 15.83487214029357659 ) ) ;
#16383 = CARTESIAN_POINT ( 'NONE',  ( 38.58424406990786082, 126.1151871740940038, 34.21067981925357060 ) ) ;
#16384 = CARTESIAN_POINT ( 'NONE',  ( 89.42064422693164261, 282.0082918409407284, 272.0939500981630204 ) ) ;
#16385 = CARTESIAN_POINT ( 'NONE',  ( 41.46631938032478359, 151.3104996726487457, 38.96596240072933170 ) ) ;
#16386 = CARTESIAN_POINT ( 'NONE',  ( 46.10157429594899270, 64.76049967264873430, 38.46393386101375711 ) ) ;
#16387 = CARTESIAN_POINT ( 'NONE',  ( 48.01140435219951996, 149.2104996726487514, 34.21067981925357060 ) ) ;
#16388 = CARTESIAN_POINT ( 'NONE',  ( 70.00144543033923128, 111.4600545017090241, 19.00928056007509070 ) ) ;
#16389 = VECTOR ( 'NONE', #1708, 1000.000000000000000 ) ;
#16390 = LINE ( 'NONE', #21482, #18498 ) ;
#16391 = ORIENTED_EDGE ( 'NONE', *, *, #7363, .T. ) ;
#16392 = LINE ( 'NONE', #12770, #10647 ) ;
#16393 = VERTEX_POINT ( 'NONE', #8335 ) ;
#16394 =( BOUNDED_CURVE ( )  B_SPLINE_CURVE ( 2, ( #5298, #12009, #6642, #13461, #18745, #15107, #11, #9832, #14882, #10161, #13352, #21628, #16861 ),
 .UNSPECIFIED., .F., .F. ) 
 B_SPLINE_CURVE_WITH_KNOTS ( ( 3, 2, 2, 2, 2, 2, 3 ),
 ( 0.05357142857142854764, 0.05714285714285714107, 0.06428571428571427937, 0.07142857142857142461, 0.07857142857142856984, 0.08571428571428571508, 0.08928571428571421831 ),
 .UNSPECIFIED. ) 
 CURVE ( )  GEOMETRIC_REPRESENTATION_ITEM ( )  RATIONAL_B_SPLINE_CURVE ( ( 0.9755282581475765991, 0.9755282581475765991, 1.000000000000000000, 0.9510565162951535312, 1.000000000000000000, 0.9510565162951535312, 1.000000000000000000, 0.9510565162951535312, 1.000000000000000000, 0.9510565162951535312, 1.000000000000000000, 0.9755282581475772652, 0.9755282581475768211 ) ) 
 REPRESENTATION_ITEM ( '' )  );
#16395 = CARTESIAN_POINT ( 'NONE',  ( 44.55648932407425633, 78.68445800887258201, 38.96596240072933170 ) ) ;
#16396 = CARTESIAN_POINT ( 'NONE',  ( 101.4021762516569822, 137.5714195593754710, 272.0939500981630204 ) ) ;
#16397 = ADVANCED_FACE ( 'NONE', ( #15047 ), #4797, .T. ) ;
#16398 = CARTESIAN_POINT ( 'NONE',  ( 48.01140435219951996, 140.3604996726487002, 32.58608133808903773 ) ) ;
#16400 = CARTESIAN_POINT ( 'NONE',  ( 23.25700774553339301, 99.89415360575743819, 9.279811863844059872 ) ) ;
#16399 = CARTESIAN_POINT ( 'NONE',  ( 38.58424406990786082, 93.11518717409400381, 34.21067981925357060 ) ) ;
#16401 = CARTESIAN_POINT ( 'NONE',  ( -120.0322075325610598, -126.9891397928655010, -54.65701158161630246 ) ) ;
#16402 = CARTESIAN_POINT ( 'NONE',  ( -145.6429501568359797, -171.2084106276440707, 41.63779006702063867 ) ) ;
#16403 = CARTESIAN_POINT ( 'NONE',  ( -159.0959885057557983, -188.1938272943107222, 44.11586579668791330 ) ) ;
#16405 = FACE_OUTER_BOUND ( 'NONE', #18586, .T. ) ;
#16404 = CARTESIAN_POINT ( 'NONE',  ( 57.67197451322198276, 240.2871645992281628, -6.999999999999982236 ) ) ;
#16406 = CARTESIAN_POINT ( 'NONE',  ( 39.92123440845005433, 105.2604996726487485, 29.95742577749336988 ) ) ;
#16407 = VECTOR ( 'NONE', #13003, 1000.000000000000000 ) ;
#16408 = CARTESIAN_POINT ( 'NONE',  ( 30.18028515090227160, 151.2280014487717779, 17.43780275515692679 ) ) ;
#16409 = CARTESIAN_POINT ( 'NONE',  ( 43.80332655382220253, 145.5373810949689926, 39.21067981925355639 ) ) ;
#16410 = VECTOR ( 'NONE', #20648, 1000.000000000000000 ) ;
#16411 = CARTESIAN_POINT ( 'NONE',  ( 46.59305225739526435, 61.31518717409399954, 36.81289934271958941 ) ) ;
#16412 = CARTESIAN_POINT ( 'NONE',  ( 72.98789752971651978, 103.3738663174133023, 6.148623012889737005 ) ) ;
#16413 = CARTESIAN_POINT ( 'NONE',  ( -148.5561028927606344, -162.9938272943107336, 58.62277379824867296 ) ) ;
#16414 = CARTESIAN_POINT ( 'NONE',  ( -142.0420953463935803, -186.8084106276440650, 52.72008163687743831 ) ) ;
#16415 = VERTEX_POINT ( 'NONE', #5242 ) ;
#16416 = CARTESIAN_POINT ( 'NONE',  ( 45.74753988029934249, 74.06518717409399244, 30.44471234641812174 ) ) ;
#16417 = CARTESIAN_POINT ( 'NONE',  ( -151.4692556286852891, -172.4084106276440309, 59.56931450028537967 ) ) ;
#16418 = CARTESIAN_POINT ( 'NONE',  ( 70.82039710638956365, 99.80338443054456832, 19.28708432993385102 ) ) ;
#16419 = SURFACE_SIDE_STYLE ('',( #3095 ) ) ;
#16420 = CARTESIAN_POINT ( 'NONE',  ( 43.01140435219951286, 135.8651871740940180, 38.86567161673127657 ) ) ;
#16421 = CARTESIAN_POINT ( 'NONE',  ( 29.91082003397629663, 88.36561978549612206, -12.22780263974880022 ) ) ;
#16422 = ORIENTED_EDGE ( 'NONE', *, *, #6462, .F. ) ;
#16423 = ORIENTED_EDGE ( 'NONE', *, *, #13738, .T. ) ;
#16424 = CARTESIAN_POINT ( 'NONE',  ( 42.37836782381873491, 91.71465960395167372, 14.44224817795539373 ) ) ;
#16425 = ORIENTED_EDGE ( 'NONE', *, *, #10773, .F. ) ;
#16426 = CARTESIAN_POINT ( 'NONE',  ( 48.01140435219951996, 116.0604996726487599, 35.83527830041809636 ) ) ;
#16427 = CARTESIAN_POINT ( 'NONE',  ( 40.27526882409969033, 71.92977050742729261, 30.44471234641811819 ) ) ;
#16429 = CARTESIAN_POINT ( 'NONE',  ( 24.25535704844963547, 98.85002770340597067, 1.227849354118501601 ) ) ;
#16428 = CARTESIAN_POINT ( 'NONE',  ( 44.37947211624943833, 130.0151871740939953, 38.42115945441014446 ) ) ;
#16430 = CARTESIAN_POINT ( 'NONE',  ( 46.10157429594899270, 91.76049967264873430, 38.46393386101376421 ) ) ;
#16431 = DIRECTION ( 'NONE',  ( 0.000000000000000000, 0.000000000000000000, 1.000000000000000000 ) ) ;
#16432 = DIRECTION ( 'NONE',  ( -1.000000000000000000, 0.000000000000000000, -0.000000000000000000 ) ) ;
#16433 = CARTESIAN_POINT ( 'NONE',  ( -151.4692556286852891, -196.9891397928655010, 39.65701158161630246 ) ) ;
#16434 = CARTESIAN_POINT ( 'NONE',  ( 40.27526882409969033, 92.66518717409398675, 30.44471234641811819 ) ) ;
#16435 = DIRECTION ( 'NONE',  ( 1.000000000000000000, 0.000000000000000000, -1.186952418100008983E-16 ) ) ;
#16436 = PRODUCT_DEFINITION_SHAPE ( 'NONE', 'NONE',  #18895 ) ;
#16437 = DIRECTION ( 'NONE',  ( -0.000000000000000000, -0.000000000000000000, -1.000000000000000000 ) ) ;
#16438 = ORIENTED_EDGE ( 'NONE', *, *, #15279, .F. ) ;
#16439 = CARTESIAN_POINT ( 'NONE',  ( 39.42975644700377558, 78.67977050742732104, 36.81289934271958941 ) ) ;
#16440 = CARTESIAN_POINT ( 'NONE',  ( -142.0420953463936087, -195.6584106276440593, 49.65701158161630957 ) ) ;
#16441 = CARTESIAN_POINT ( 'NONE',  ( 14.15704070161504369, 138.3271338521546454, 9.720138693322796897 ) ) ;
#16442 = CARTESIAN_POINT ( 'NONE',  ( -157.2955611005346270, -182.6084106276440480, 41.63779006702063867 ) ) ;
#16443 = ORIENTED_EDGE ( 'NONE', *, *, #3591, .T. ) ;
#16444 = CARTESIAN_POINT ( 'NONE',  ( -153.0531000319306827, -162.1622583705451461, 39.65701158161629536 ) ) ;
#16445 = ADVANCED_FACE ( 'NONE', ( #20348 ), #17129, .T. ) ;
#16446 = DIRECTION ( 'NONE',  ( 1.000000000000000000, 0.000000000000000000, 0.000000000000000000 ) ) ;
#16447 = CARTESIAN_POINT ( 'NONE',  ( 44.37947211624943833, 128.4797705074273040, 30.00020018409699318 ) ) ;
#16448 = EDGE_LOOP ( 'NONE', ( #2124, #11163, #2667, #16811 ) ) ;
#16449 = CARTESIAN_POINT ( 'NONE',  ( 48.01140435219951996, 130.1344580088725422, 35.83527830041809636 ) ) ;
#16450 = ORIENTED_EDGE ( 'NONE', *, *, #15541, .F. ) ;
#16451 = CIRCLE ( 'NONE', #1682, 24.99999999999998934 ) ;
#16452 = CARTESIAN_POINT ( 'NONE',  ( 43.01140435219954838, 132.5344580088725763, 39.21067981925356349 ) ) ;
#16453 = CARTESIAN_POINT ( 'NONE',  ( 38.58424406990786082, 90.37977050742732388, 34.21067981925357060 ) ) ;
#16454 = CARTESIAN_POINT ( 'NONE',  ( 45.51146558786459195, 58.78519036379218221, 29.88058815533641166 ) ) ;
#16455 = CARTESIAN_POINT ( 'NONE',  ( 107.0370895198517189, 343.6663954850758955, -19.99999999999997868 ) ) ;
#16456 = FACE_OUTER_BOUND ( 'NONE', #19070, .T. ) ;
#16457 = LINE ( 'NONE', #5995, #17567 ) ;
#16458 = CARTESIAN_POINT ( 'NONE',  ( -161.4692556286852607, -191.3391397928654669, 52.90620854394536821 ) ) ;
#16459 = CARTESIAN_POINT ( 'NONE',  ( 42.21948215057684450, 89.11133943119283174, 29.21067981925356705 ) ) ;
#16460 = DIRECTION ( 'NONE',  ( 0.000000000000000000, 0.000000000000000000, 1.000000000000000000 ) ) ;
#16461 = CARTESIAN_POINT ( 'NONE',  ( -143.8425227516148084, -192.0938272943107279, 44.11586579668791330 ) ) ;
#16462 = CONTEXT_DEPENDENT_SHAPE_REPRESENTATION ( #2526, #4655 ) ;
#16463 = CARTESIAN_POINT ( 'NONE',  ( 38.01140435219952707, 119.7844580088725763, 34.21067981925357060 ) ) ;
#16464 = CARTESIAN_POINT ( 'NONE',  ( 39.42975644700377558, 105.0797705074273125, 31.60846029578754468 ) ) ;
#16465 = CARTESIAN_POINT ( 'NONE',  ( 24.99951789580824268, 141.7104366081036346, 16.15213770299339657 ) ) ;
#16466 = CARTESIAN_POINT ( 'NONE',  ( -157.2955611005346270, -181.4438272943107506, 57.67623309621198047 ) ) ;
#16467 = CARTESIAN_POINT ( 'NONE',  ( 46.59305225739526435, 85.31518717409400665, 36.81289934271958941 ) ) ;
#16468 = CYLINDRICAL_SURFACE ( 'NONE', #16038, 4.999999999999997335 ) ;
#16469 = ORIENTED_EDGE ( 'NONE', *, *, #3855, .F. ) ;
#16470 = DIRECTION ( 'NONE',  ( 0.000000000000000000, 1.000000000000000000, 0.000000000000000000 ) ) ;
#16471 = CARTESIAN_POINT ( 'NONE',  ( 18.14018356548558941, 143.3940520581896862, 16.92415443696469879 ) ) ;
#16472 = CARTESIAN_POINT ( 'NONE',  ( 15.18239976710701100, 124.4615124019231018, 16.34704286353642999 ) ) ;
#16473 = CARTESIAN_POINT ( 'NONE',  ( 41.64333658814960870, 62.77977050742732246, 30.00020018409699318 ) ) ;
#16474 = ORIENTED_EDGE ( 'NONE', *, *, #11473, .F. ) ;
#16475 = ORIENTED_EDGE ( 'NONE', *, *, #2604, .T. ) ;
#16476 = CARTESIAN_POINT ( 'NONE',  ( 39.42975644700377558, 144.0797705074273267, 31.60846029578754468 ) ) ;
#16477 = ADVANCED_FACE ( 'NONE', ( #10640 ), #8773, .T. ) ;
#16479 = EDGE_CURVE ( 'NONE', #5574, #14220, #2251, .T. ) ;
#16478 = DIRECTION ( 'NONE',  ( 0.000000000000000000, -0.000000000000000000, 1.000000000000000000 ) ) ;
#16480 = CARTESIAN_POINT ( 'NONE',  ( 46.10157429594899270, 110.6604996726487400, 29.95742577749337343 ) ) ;
#16481 = CARTESIAN_POINT ( 'NONE',  ( 47.43856463449117200, 70.46518717409401233, 35.64915139335016647 ) ) ;
#16482 = FACE_OUTER_BOUND ( 'NONE', #19308, .T. ) ;
#16483 = CARTESIAN_POINT ( 'NONE',  ( -145.6429501568359797, -158.9438272943107222, 41.63779006702063867 ) ) ;
#16484 = FACE_OUTER_BOUND ( 'NONE', #16890, .T. ) ;
#16485 = CARTESIAN_POINT ( 'NONE',  ( -141.4692556286852891, -174.0630981290893260, 49.65701158161630957 ) ) ;
#16486 = CARTESIAN_POINT ( 'NONE',  ( 47.05648932407426344, 151.5844580088725877, 31.27175355779120025 ) ) ;
#16487 = CARTESIAN_POINT ( 'NONE',  ( 38.58424406990784661, 132.5297705074272869, 35.64915139335016647 ) ) ;
#16488 = CARTESIAN_POINT ( 'NONE',  ( 55.77169822954404310, 151.7599422098969910, 17.26344356872107255 ) ) ;
#16489 = CARTESIAN_POINT ( 'NONE',  ( 46.59305225739526435, 115.3151871740940067, 36.81289934271958941 ) ) ;
#16490 = LINE ( 'NONE', #8474, #9368 ) ;
#16491 = CARTESIAN_POINT ( 'NONE',  ( -130.4480969619998234, -126.9891397928655010, 67.64809332337415526 ) ) ;
#16492 = CARTESIAN_POINT ( 'NONE',  ( 46.10157429594899270, 140.6604996726487116, 29.95742577749336988 ) ) ;
#16493 = CARTESIAN_POINT ( 'NONE',  ( 31.96084264191244273, 87.59053552682176758, 1.700516636338098797 ) ) ;
#16494 = CARTESIAN_POINT ( 'NONE',  ( 43.06284635655732274, 148.1064719378950088, -10.08176808973812655 ) ) ;
#16495 = CARTESIAN_POINT ( 'NONE',  ( 43.01140435219951286, 119.9604996726487229, 29.21067981925356705 ) ) ;
#16496 = EDGE_CURVE ( 'NONE', #17982, #21732, #20773, .T. ) ;
#16497 = VECTOR ( 'NONE', #70, 1000.000000000000000 ) ;
#16498 = CARTESIAN_POINT ( 'NONE',  ( 44.37947211624943833, 91.27977050742731535, 38.42115945441014446 ) ) ;
#16499 = ORIENTED_EDGE ( 'NONE', *, *, #3722, .T. ) ;
#16500 = CARTESIAN_POINT ( 'NONE',  ( 53.01140435219953417, 119.9070776186055838, -19.99999999999997868 ) ) ;
#16501 = ORIENTED_EDGE ( 'NONE', *, *, #11961, .T. ) ;
#16502 = CARTESIAN_POINT ( 'NONE',  ( 38.01140435219951996, 86.93445800887258201, 35.83527830041810347 ) ) ;
#16503 = CARTESIAN_POINT ( 'NONE',  ( 91.17254549292282206, -61.68114226949890622, -16.21320343559643717 ) ) ;
#16504 = CARTESIAN_POINT ( 'NONE',  ( 46.10157429594899270, 137.6604996726487116, 29.95742577749337343 ) ) ;
#16506 = CARTESIAN_POINT ( 'NONE',  ( 14.94553207812311690, 121.6546367895698779, 10.23235069918434981 ) ) ;
#16505 = CARTESIAN_POINT ( 'NONE',  ( 43.01140435219951286, 98.36518717409401802, 29.55568802177586463 ) ) ;
#16507 = LINE ( 'NONE', #11971, #9509 ) ;
#16508 = CARTESIAN_POINT ( 'NONE',  ( -159.0959885057557983, -164.4584106276440423, 44.11586579668791330 ) ) ;
#16509 = CARTESIAN_POINT ( 'NONE',  ( -142.0420953463936087, -189.3938272943107393, 49.65701158161630957 ) ) ;
#16511 = LINE ( 'NONE', #6498, #2332 ) ;
#16510 = CARTESIAN_POINT ( 'NONE',  ( -153.0531000319306827, -165.8899795514095672, 59.65701158161631668 ) ) ;
#16512 = DIRECTION ( 'NONE',  ( 1.000000000000000000, 0.000000000000000000, 0.000000000000000000 ) ) ;
#16513 = CARTESIAN_POINT ( 'NONE',  ( -141.4692556286852891, -175.1391397928654783, 52.90620854394536821 ) ) ;
#16514 = CARTESIAN_POINT ( 'NONE',  ( 121.4021762516569964, 137.5714195593754710, -19.99999999999997868 ) ) ;
#16515 = CARTESIAN_POINT ( 'NONE',  ( 38.58424406990784661, 159.2297705074272756, 32.77220824515698183 ) ) ;
#16516 = CARTESIAN_POINT ( 'NONE',  ( 44.55648932407425633, 157.6104996726487570, 38.96596240072933170 ) ) ;
#16517 = CARTESIAN_POINT ( 'NONE',  ( 73.32203938827501588, 103.9946350594383517, -0.8753108214479579097 ) ) ;
#16518 = CARTESIAN_POINT ( 'NONE',  ( 44.37947211624943833, 148.0151871740940237, 38.42115945441014446 ) ) ;
#16519 = CARTESIAN_POINT ( 'NONE',  ( -159.0959885057557983, -161.1938272943107222, 44.11586579668791330 ) ) ;
#16520 = CARTESIAN_POINT ( 'NONE',  ( -151.4692556286852891, -187.4084106276440309, 59.56931450028537256 ) ) ;
#16521 = ORIENTED_EDGE ( 'NONE', *, *, #7326, .F. ) ;
#16522 = CARTESIAN_POINT ( 'NONE',  ( 47.43856463449118621, 73.61518717409400381, 34.21067981925357060 ) ) ;
#16523 = CARTESIAN_POINT ( 'NONE',  ( -143.8425227516148084, -168.3584106276440480, 44.11586579668791330 ) ) ;
#16524 = CARTESIAN_POINT ( 'NONE',  ( 73.69864372527810303, 135.2613471474284097, 11.07306444099484466 ) ) ;
#16525 = CARTESIAN_POINT ( 'NONE',  ( 44.37947211624943833, 121.0151871740940095, 38.42115945441014446 ) ) ;
#16526 = ADVANCED_FACE ( 'NONE', ( #18690 ), #492, .T. ) ;
#16527 = CARTESIAN_POINT ( 'NONE',  ( 71.68162264554656815, 101.3460857334412708, -13.77530061520655025 ) ) ;
#16528 =( BOUNDED_CURVE ( )  B_SPLINE_CURVE ( 2, ( #15182, #1297, #8031, #13421, #21586, #1407, #16604, #6597, #1626, #6252, #12982, #6714, #8359 ),
 .UNSPECIFIED., .F., .F. ) 
 B_SPLINE_CURVE_WITH_KNOTS ( ( 3, 2, 2, 2, 2, 2, 3 ),
 ( 0.6607142857142856984, 0.6642857142857142572, 0.6714285714285713746, 0.6785714285714286031, 0.6857142857142857206, 0.6928571428571428381, 0.6964285714285713969 ),
 .UNSPECIFIED. ) 
 CURVE ( )  GEOMETRIC_REPRESENTATION_ITEM ( )  RATIONAL_B_SPLINE_CURVE ( ( 0.9755282581475768211, 0.9755282581475768211, 1.000000000000000000, 0.9510565162951535312, 1.000000000000000000, 0.9510565162951535312, 1.000000000000000000, 0.9510565162951535312, 1.000000000000000000, 0.9510565162951535312, 1.000000000000000000, 0.9755282581475768211, 0.9755282581475768211 ) ) 
 REPRESENTATION_ITEM ( '' )  );
#16529 = ORIENTED_EDGE ( 'NONE', *, *, #2728, .F. ) ;
#16530 = VERTEX_POINT ( 'NONE', #18899 ) ;
#16531 = AXIS2_PLACEMENT_3D ( 'NONE', #3712, #10760, #13623 ) ;
#16532 = CARTESIAN_POINT ( 'NONE',  ( 38.01140435219952707, 113.7844580088725763, 34.21067981925357060 ) ) ;
#16533 = EDGE_LOOP ( 'NONE', ( #6180, #766 ) ) ;
#16534 = CARTESIAN_POINT ( 'NONE',  ( 43.01140435219951286, 107.0344580088725905, 28.95336869806222779 ) ) ;
#16535 = DIRECTION ( 'NONE',  ( 0.5010362705417042983, 0.000000000000000000, 0.8654262854811264338 ) ) ;
#16536 = CARTESIAN_POINT ( 'NONE',  ( 38.58424406990784661, 69.52977050742730114, 35.64915139335016647 ) ) ;
#16538 = CARTESIAN_POINT ( 'NONE',  ( 17.48807464456866256, 131.8965856249792523, 2.656420782620954935 ) ) ;
#16537 = CARTESIAN_POINT ( 'NONE',  ( 38.58424406990784661, 126.2651871740940237, 35.64915139335016647 ) ) ;
#16539 = CARTESIAN_POINT ( 'NONE',  ( 48.01140435219951996, 80.21049967264875136, 34.21067981925357060 ) ) ;
#16540 = CARTESIAN_POINT ( 'NONE',  ( 30.18028515090226449, 151.2280014487717779, 17.43780275515692679 ) ) ;
#16541 = CARTESIAN_POINT ( 'NONE',  ( 43.01140435219951286, 145.4604996726487229, 39.21067981925356349 ) ) ;
#16542 = CARTESIAN_POINT ( 'NONE',  ( -23.27144139456156324, -18.88988604584387332, 4.000000000000021316 ) ) ;
#16543 = CARTESIAN_POINT ( 'NONE',  ( 47.43856463449118621, 91.61518717409400381, 34.21067981925357060 ) ) ;
#16544 = CARTESIAN_POINT ( 'NONE',  ( 43.80332655382220253, 150.6113394311928460, 39.21067981925355639 ) ) ;
#16545 = CYLINDRICAL_SURFACE ( 'NONE', #21183, 4.999999999999997335 ) ;
#16546 =( GEOMETRIC_REPRESENTATION_CONTEXT ( 3 ) GLOBAL_UNCERTAINTY_ASSIGNED_CONTEXT ( ( #12372 ) ) GLOBAL_UNIT_ASSIGNED_CONTEXT ( ( #8827, #15535, #7062 ) ) REPRESENTATION_CONTEXT ( 'NONE', 'WORKASPACE' ) );
#16547 = EDGE_LOOP ( 'NONE', ( #1216, #7772, #20967, #11217 ) ) ;
#16548 = CARTESIAN_POINT ( 'NONE',  ( 45.74753988029933538, 62.32977050742730540, 30.44471234641811819 ) ) ;
#16549 = CARTESIAN_POINT ( 'NONE',  ( -142.0420953463935803, -156.5438272943107165, 52.72008163687743831 ) ) ;
#16550 = CARTESIAN_POINT ( 'NONE',  ( 67.39040179371399120, 143.9404232637865562, 4.720051584306741432 ) ) ;
#16551 = EDGE_CURVE ( 'NONE', #20722, #9507, #13825, .T. ) ;
#16552 = CARTESIAN_POINT ( 'NONE',  ( -154.3824083646099439, -187.5584106276440650, 58.62277379824867296 ) ) ;
#16553 = ORIENTED_EDGE ( 'NONE', *, *, #5276, .F. ) ;
#16554 = CARTESIAN_POINT ( 'NONE',  ( 39.42975644700377558, 156.4151871740940010, 36.81289934271958941 ) ) ;
#16555 = DIRECTION ( 'NONE',  ( 0.000000000000000000, 1.000000000000000000, 0.000000000000000000 ) ) ;
#16556 = CARTESIAN_POINT ( 'NONE',  ( 44.37947211624943833, 113.4797705074273324, 30.00020018409699318 ) ) ;
#16557 = CARTESIAN_POINT ( 'NONE',  ( 74.62708615766334219, 133.0342049366344384, -8.851289726714327344 ) ) ;
#16558 = ORIENTED_EDGE ( 'NONE', *, *, #3467, .F. ) ;
#16559 = EDGE_LOOP ( 'NONE', ( #5026, #682 ) ) ;
#16560 = CARTESIAN_POINT ( 'NONE',  ( 47.43856463449117200, 115.7297705074273324, 35.64915139335016647 ) ) ;
#16561 = LINE ( 'NONE', #2797, #14304 ) ;
#16562 = CARTESIAN_POINT ( 'NONE',  ( 45.05632365893699642, 58.83593307231945602, 29.61780325802818226 ) ) ;
#16563 = DIRECTION ( 'NONE',  ( -0.000000000000000000, -0.000000000000000000, 1.000000000000000000 ) ) ;
#16564 = CARTESIAN_POINT ( 'NONE',  ( 41.46631938032478359, 83.18445800887258201, 29.45539723777780239 ) ) ;
#16565 = DIRECTION ( 'NONE',  ( -0.000000000000000000, -0.000000000000000000, -1.000000000000000000 ) ) ;
#16566 = CARTESIAN_POINT ( 'NONE',  ( -143.3790856849358306, -178.2891397928654840, 55.53486410454105027 ) ) ;
#16567 = CARTESIAN_POINT ( 'NONE',  ( 39.92123440845005433, 157.1604996726487400, 38.46393386101375711 ) ) ;
#16568 = CARTESIAN_POINT ( 'NONE',  ( 48.01140435219951996, 94.13445800887258486, 35.83527830041809636 ) ) ;
#16569 = CARTESIAN_POINT ( 'NONE',  ( -154.3824083646099439, -188.4938272943107336, 40.69124936498395328 ) ) ;
#16570 = CONTEXT_DEPENDENT_SHAPE_REPRESENTATION ( #6772, #11156 ) ;
#16571 = CARTESIAN_POINT ( 'NONE',  ( 47.05648932407426344, 127.5844580088725877, 31.27175355779120025 ) ) ;
#16572 = CARTESIAN_POINT ( 'NONE',  ( 39.42975644700377558, 93.07977050742731251, 31.60846029578754468 ) ) ;
#16573 = CARTESIAN_POINT ( 'NONE',  ( 65.96530660583994177, 103.3855952397044007, 19.36639486037446289 ) ) ;
#16574 = CARTESIAN_POINT ( 'NONE',  ( -142.0420953463936087, -186.3938272943107393, 49.65701158161630957 ) ) ;
#16575 = CARTESIAN_POINT ( 'NONE',  ( 44.37947211624943833, 88.01518717409399528, 38.42115945441014446 ) ) ;
#16576 = CARTESIAN_POINT ( 'NONE',  ( 38.96631938032478359, 85.01049967264874851, 37.14960608071593384 ) ) ;
#16577 = ORIENTED_EDGE ( 'NONE', *, *, #161, .F. ) ;
#16578 = CYLINDRICAL_SURFACE ( 'NONE', #17158, 4.999999999999997335 ) ;
#16579 = CARTESIAN_POINT ( 'NONE',  ( 14.48810111090402941, 100.9784058478479523, 15.43442115621699529 ) ) ;
#16580 = CARTESIAN_POINT ( 'NONE',  ( 69.09677972725788209, 109.4046064338026127, -6.910527774811301427 ) ) ;
#16581 = CARTESIAN_POINT ( 'NONE',  ( 40.27526882409969033, 104.6651871740939868, 30.44471234641811819 ) ) ;
#16582 = ADVANCED_FACE ( 'NONE', ( #8664 ), #11959, .T. ) ;
#16583 = CARTESIAN_POINT ( 'NONE',  ( 40.27526882409969744, 68.92977050742732104, 30.44471234641812174 ) ) ;
#16584 = EDGE_LOOP ( 'NONE', ( #2650, #2221, #17742, #19223, #5057, #21764, #6085, #14242 ) ) ;
#16585 = CARTESIAN_POINT ( 'NONE',  ( 43.01140435219951286, 143.6297705074272812, 29.55568802177586463 ) ) ;
#16586 = VECTOR ( 'NONE', #20564, 1000.000000000000000 ) ;
#16587 = CARTESIAN_POINT ( 'NONE',  ( 39.42975644700377558, 99.07977050742732672, 31.60846029578754468 ) ) ;
#16588 = PLANE ( 'NONE',  #11950 ) ;
#16589 = PRODUCT_DEFINITION ( 'UNKNOWN', '', #19358, #1791 ) ;
#16590 = CARTESIAN_POINT ( 'NONE',  ( 41.46631938032478359, 106.3104996726487457, 38.96596240072933170 ) ) ;
#16591 = CARTESIAN_POINT ( 'NONE',  ( 47.43856463449118621, 70.61518717409400381, 34.21067981925357060 ) ) ;
#16592 = CARTESIAN_POINT ( 'NONE',  ( 147.8787791192428074, -126.9891397928655010, 39.65701158161628825 ) ) ;
#16593 = CARTESIAN_POINT ( 'NONE',  ( -160.8964159109769696, -157.7438272943107336, 52.72008163687743121 ) ) ;
#16594 = DIRECTION ( 'NONE',  ( 0.000000000000000000, 0.000000000000000000, 1.000000000000000000 ) ) ;
#16595 = CARTESIAN_POINT ( 'NONE',  ( -145.2889157411863721, -182.6130981290893374, 41.15050349809590102 ) ) ;
#16596 = CARTESIAN_POINT ( 'NONE',  ( 0.000000000000000000, 0.000000000000000000, 0.000000000000000000 ) ) ;
#16597 = DIRECTION ( 'NONE',  ( -0.000000000000000000, 1.000000000000000000, -0.000000000000000000 ) ) ;
#16598 = EDGE_CURVE ( 'NONE', #9959, #8850, #12934, .T. ) ;
#16599 = CARTESIAN_POINT ( 'NONE',  ( 38.01140435219951996, 152.9344580088725536, 35.83527830041810347 ) ) ;
#16600 = CARTESIAN_POINT ( 'NONE',  ( 45.74753988029933538, 133.4297705074273210, 37.97664729208901946 ) ) ;
#16601 = CARTESIAN_POINT ( 'NONE',  ( 74.43934690056714487, 106.1333445020626129, 19.04903893889577660 ) ) ;
#16602 = B_SPLINE_CURVE_WITH_KNOTS ( 'NONE', 3,
 ( #9568, #9894, #21466, #4699, #6707, #18142, #11534, #16274 ),
 .UNSPECIFIED., .F., .F.,
 ( 4, 2, 2, 4 ),
 ( 3.469446951953614189E-18, 0.001432241572422958973, 0.002148362358634439868, 0.002864483144845920981 ),
 .UNSPECIFIED. ) ;
#16603 = CARTESIAN_POINT ( 'NONE',  ( 47.43856463449117911, 118.7651871740940237, 32.77220824515697473 ) ) ;
#16604 = CARTESIAN_POINT ( 'NONE',  ( -161.4692556286853176, -167.4891397928654726, 49.65701158161630957 ) ) ;
#16605 = AXIS2_PLACEMENT_3D ( 'NONE', #6980, #3556, #136 ) ;
#16606 = DIRECTION ( 'NONE',  ( -0.000000000000000000, -0.000000000000000000, 1.000000000000000000 ) ) ;
#16607 = CARTESIAN_POINT ( 'NONE',  ( 43.80332655382220253, 65.88361825032846752, 29.21067981925356705 ) ) ;
#16608 = CARTESIAN_POINT ( 'NONE',  ( 62.62098228421420032, 91.94359626243755201, 7.653270806628301948 ) ) ;
#16609 = EDGE_CURVE ( 'NONE', #16234, #8233, #4017, .T. ) ;
#16610 = CARTESIAN_POINT ( 'NONE',  ( 15.00983914341701997, 123.2415857317943448, 2.299110145932334426 ) ) ;
#16611 = FACE_OUTER_BOUND ( 'NONE', #7192, .T. ) ;
#16612 = VECTOR ( 'NONE', #19619, 1000.000000000000000 ) ;
#16613 = CARTESIAN_POINT ( 'NONE',  ( 47.43856463449117911, 94.72977050742733240, 35.64915139335015937 ) ) ;
#16614 = ORIENTED_EDGE ( 'NONE', *, *, #2767, .T. ) ;
#16615 = EDGE_CURVE ( 'NONE', #13269, #17319, #5664, .T. ) ;
#16616 = ORIENTED_EDGE ( 'NONE', *, *, #3264, .F. ) ;
#16617 = CARTESIAN_POINT ( 'NONE',  ( 48.01140435219951996, 85.13445800887258486, 35.83527830041810347 ) ) ;
#16618 = DIRECTION ( 'NONE',  ( 0.000000000000000000, 0.000000000000000000, -1.000000000000000000 ) ) ;
#16619 = PRODUCT_DEFINITION_SHAPE ( 'NONE', 'NONE',  #17263 ) ;
#16620 = CARTESIAN_POINT ( 'NONE',  ( 38.96631938032478359, 135.4104996726487400, 31.27175355779120025 ) ) ;
#16622 = CARTESIAN_POINT ( 'NONE',  ( 45.76500403897348690, 91.92250713676531859, 1.303787141088997181 ) ) ;
#16621 = CARTESIAN_POINT ( 'NONE',  ( 38.58424406990784661, 98.96518717409398391, 32.77220824515698183 ) ) ;
#16623 = DIRECTION ( 'NONE',  ( 0.000000000000000000, 1.000000000000000000, 0.000000000000000000 ) ) ;
#16624 = CARTESIAN_POINT ( 'NONE',  ( -160.8964159109769696, -167.3084106276440366, 46.59394152635518793 ) ) ;
#16625 = CARTESIAN_POINT ( 'NONE',  ( -157.2955611005345986, -187.4438272943106938, 57.67623309621197336 ) ) ;
#16627 = CARTESIAN_POINT ( 'NONE',  ( -151.4692556286852607, -166.7391397928654442, 59.65701158161632378 ) ) ;
#16626 = LINE ( 'NONE', #9704, #3774 ) ;
#16628 = ADVANCED_BREP_SHAPE_REPRESENTATION ( '', ( #21708, #12657 ), #1776 ) ;
#16629 = CARTESIAN_POINT ( 'NONE',  ( 39.92123440845005433, 148.1604996726487400, 38.46393386101375711 ) ) ;
#16630 = CARTESIAN_POINT ( 'NONE',  ( 47.05648932407426344, 145.9104996726487400, 37.14960608071593384 ) ) ;
#16631 = CARTESIAN_POINT ( 'NONE',  ( 39.42975644700377558, 62.81518717409399954, 31.60846029578754468 ) ) ;
#16632 = LINE ( 'NONE', #8384, #12593 ) ;
#16633 = CARTESIAN_POINT ( 'NONE',  ( 73.40451243997107156, 135.6611253642151098, -1.946480675884423084 ) ) ;
#16634 = CARTESIAN_POINT ( 'NONE',  ( 41.64333658814960870, 149.5151871740940237, 30.00020018409699318 ) ) ;
#16635 = CARTESIAN_POINT ( 'NONE',  ( -142.0420953463935803, -159.5438272943107449, 52.72008163687743831 ) ) ;
#16636 = CARTESIAN_POINT ( 'NONE',  ( -154.3824083646099439, -172.5584106276440366, 58.62277379824867296 ) ) ;
#16637 = ADVANCED_FACE ( 'NONE', ( #20453 ), #3592, .T. ) ;
#16638 = ORIENTED_EDGE ( 'NONE', *, *, #13631, .T. ) ;
#16639 = CARTESIAN_POINT ( 'NONE',  ( 43.01140435219951286, 77.03445800887257633, 29.21067981925356705 ) ) ;
#16640 = CARTESIAN_POINT ( 'NONE',  ( -151.4692556286852891, -157.4084106276440593, 59.56931450028537967 ) ) ;
#16641 = CARTESIAN_POINT ( 'NONE',  ( 9.691656460246418803, 128.1079710775123601, 15.35877872671195910 ) ) ;
#16642 = CARTESIAN_POINT ( 'NONE',  ( 48.01140435219951996, 112.4344580088725536, 32.58608133808903773 ) ) ;
#16643 = CARTESIAN_POINT ( 'NONE',  ( 44.37947211624943833, 122.2151871740940123, 30.00020018409699318 ) ) ;
#16644 = CARTESIAN_POINT ( 'NONE',  ( 9.647618190908266556, 112.6042302384299916, -11.15662622088235167 ) ) ;
#16645 = EDGE_LOOP ( 'NONE', ( #19149, #7446, #631, #18609 ) ) ;
#16646 = ORIENTED_EDGE ( 'NONE', *, *, #9067, .T. ) ;
#16647 = DIRECTION ( 'NONE',  ( 0.9385982292947087080, 0.3450121214752279175, -0.000000000000000000 ) ) ;
#16648 = VERTEX_POINT ( 'NONE', #12388 ) ;
#16649 = CARTESIAN_POINT ( 'NONE',  ( 44.37947211624943833, 157.2797705074273438, 38.42115945441014446 ) ) ;
#16650 = CARTESIAN_POINT ( 'NONE',  ( 44.37947211624943833, 64.27977050742731535, 38.42115945441014446 ) ) ;
#16652 = CARTESIAN_POINT ( 'NONE',  ( 55.20039838223064521, 94.47806301326188816, -0.08174959847185196693 ) ) ;
#16651 = CARTESIAN_POINT ( 'NONE',  ( 43.01140435219951286, 123.8651871740939896, 38.86567161673127657 ) ) ;
#16653 = CARTESIAN_POINT ( 'NONE',  ( 38.01140435219951996, 84.56049967264871725, 32.58608133808903773 ) ) ;
#16654 = CARTESIAN_POINT ( 'NONE',  ( -151.4692556286852607, -162.2391397928654442, 39.65701158161629536 ) ) ;
#16655 = EDGE_CURVE ( 'NONE', #16987, #6094, #1089, .T. ) ;
#16656 = CARTESIAN_POINT ( 'NONE',  ( -145.2889157411863437, -171.5130981290893146, 58.16351966513671812 ) ) ;
#16657 = CARTESIAN_POINT ( 'NONE',  ( 38.96631938032478359, 138.4104996726487400, 31.27175355779120025 ) ) ;
#16658 = CARTESIAN_POINT ( 'NONE',  ( 40.27526882409969033, 86.66518717409400097, 30.44471234641811819 ) ) ;
#16659 = CARTESIAN_POINT ( 'NONE',  ( 38.01140435219952707, 81.71049967264873715, 34.21067981925357060 ) ) ;
#16660 = CARTESIAN_POINT ( 'NONE',  ( 42.21948215057684450, 133.3836182503284533, 39.21067981925356349 ) ) ;
#16661 = ORIENTED_EDGE ( 'NONE', *, *, #6688, .T. ) ;
#16662 = CARTESIAN_POINT ( 'NONE',  ( 45.74753988029933538, 68.32977050742731251, 30.44471234641811819 ) ) ;
#16663 =( BOUNDED_CURVE ( )  B_SPLINE_CURVE ( 2, ( #19185, #14321, #21063, #10813, #17516, #12674, #2425, #19394, #4291, #11018, #17729, #2634, #16080 ),
 .UNSPECIFIED., .F., .T. ) 
 B_SPLINE_CURVE_WITH_KNOTS ( ( 3, 2, 2, 2, 2, 2, 3 ),
 ( 0.9485294117647058432, 0.9499999999999999556, 0.9529411764705881804, 0.9558823529411765163, 0.9588235294117647411, 0.9617647058823529660, 0.9632352941176470784 ),
 .UNSPECIFIED. ) 
 CURVE ( )  GEOMETRIC_REPRESENTATION_ITEM ( )  RATIONAL_B_SPLINE_CURVE ( ( 0.9755282581475768211, 0.9755282581475768211, 1.000000000000000000, 0.9510565162951535312, 1.000000000000000000, 0.9510565162951535312, 1.000000000000000000, 0.9510565162951535312, 1.000000000000000000, 0.9510565162951535312, 1.000000000000000000, 0.9755282581475768211, 0.9755282581475768211 ) ) 
 REPRESENTATION_ITEM ( '' )  );
#16664 = CARTESIAN_POINT ( 'NONE',  ( -160.8964159109769696, -188.0084106276440252, 52.72008163687743121 ) ) ;
#16665 = CARTESIAN_POINT ( 'NONE',  ( 17.60877916486148465, 96.95950790538488206, 1.267834678905774393 ) ) ;
#16666 = CARTESIAN_POINT ( 'NONE',  ( -160.8964159109769696, -185.3084106276440082, 46.59394152635518793 ) ) ;
#16667 = ORIENTED_EDGE ( 'NONE', *, *, #9958, .T. ) ;
#16668 = CARTESIAN_POINT ( 'NONE',  ( 43.01140435219951286, 149.3651871740939612, 29.55568802177586463 ) ) ;
#16669 = DIRECTION ( 'NONE',  ( -0.9385982292947088190, -0.3450121214752278620, 0.000000000000000000 ) ) ;
#16670 = CARTESIAN_POINT ( 'NONE',  ( 47.43856463449117911, 113.0297705074273154, 32.77220824515697473 ) ) ;
#16671 = CARTESIAN_POINT ( 'NONE',  ( 8.779377865064803999, 119.6051361893432130, -4.922546661887801100 ) ) ;
#16672 = VERTEX_POINT ( 'NONE', #2147 ) ;
#16673 = CARTESIAN_POINT ( 'NONE',  ( 44.18632541912793243, 91.73153706005567187, -6.629209314582290347 ) ) ;
#16674 = VERTEX_POINT ( 'NONE', #8880 ) ;
#16675 = CARTESIAN_POINT ( 'NONE',  ( 38.58424406990784661, 114.2297705074273040, 32.77220824515698183 ) ) ;
#16676 = CARTESIAN_POINT ( 'NONE',  ( 151.4773229304660731, 84.89323405393692212, 14.00000000000001776 ) ) ;
#16677 = CARTESIAN_POINT ( 'NONE',  ( 44.37947211624943833, 151.0151871740940237, 38.42115945441014446 ) ) ;
#16678 = EDGE_CURVE ( 'NONE', #15135, #17794, #20881, .T. ) ;
#16679 = CARTESIAN_POINT ( 'NONE',  ( 63.55746018358933469, 147.2895578332197033, -9.446739241148069510 ) ) ;
#16680 = CARTESIAN_POINT ( 'NONE',  ( 23.10700517764655260, 139.6571016847272801, -10.96257334342637435 ) ) ;
#16681 = DIRECTION ( 'NONE',  ( 0.000000000000000000, -1.000000000000000000, 0.000000000000000000 ) ) ;
#16682 = LINE ( 'NONE', #20227, #11687 ) ;
#16683 = CARTESIAN_POINT ( 'NONE',  ( -161.4692556286852607, -176.6391397928654783, 46.40781461928724383 ) ) ;
#16684 = FACE_OUTER_BOUND ( 'NONE', #18528, .T. ) ;
#16685 = PLANE ( 'NONE',  #7961 ) ;
#16686 = CARTESIAN_POINT ( 'NONE',  ( 43.80332655382220253, 77.88361825032845331, 29.21067981925356705 ) ) ;
#16687 = PRODUCT_CONTEXT ( 'NONE', #1409, 'mechanical' ) ;
#16688 = CARTESIAN_POINT ( 'NONE',  ( 45.74753988029933538, 92.32977050742731251, 30.44471234641811819 ) ) ;
#16689 = CARTESIAN_POINT ( 'NONE',  ( 15.78326802858598299, 112.2624592280589439, 21.86641499745291028 ) ) ;
#16690 = CARTESIAN_POINT ( 'NONE',  ( -151.4692556286852891, -184.1438272943107108, 59.56931450028537967 ) ) ;
#16691 = AXIS2_PLACEMENT_3D ( 'NONE', #14619, #12757, #17493 ) ;
#16692 = ADVANCED_FACE ( 'NONE', ( #19539 ), #17989, .T. ) ;
#16693 = CARTESIAN_POINT ( 'NONE',  ( 38.01140435219952707, 84.71049967264873715, 34.21067981925357060 ) ) ;
#16694 = VERTEX_POINT ( 'NONE', #12498 ) ;
#16695 = CARTESIAN_POINT ( 'NONE',  ( -148.3790856849358306, -190.5891397928654953, 59.16757674456786020 ) ) ;
#16696 = CARTESIAN_POINT ( 'NONE',  ( 9.822352152143091431, 128.2981216602131553, 9.363167623699879982 ) ) ;
#16697 = CARTESIAN_POINT ( 'NONE',  ( 47.43856463449117911, 139.7297705074273324, 35.64915139335015937 ) ) ;
#16698 = CARTESIAN_POINT ( 'NONE',  ( 33.89447768034496278, 93.30632465966320410, 1.780072726204736000 ) ) ;
#16699 = EDGE_CURVE ( 'NONE', #2116, #13398, #17878, .T. ) ;
#16700 = CARTESIAN_POINT ( 'NONE',  ( 38.58424406990785371, 60.52977050742731535, 35.64915139335015937 ) ) ;
#16701 = ORIENTED_EDGE ( 'NONE', *, *, #5344, .F. ) ;
#16702 = CARTESIAN_POINT ( 'NONE',  ( 41.64333658814960870, 146.7797705074273154, 30.00020018409699318 ) ) ;
#16703 = CARTESIAN_POINT ( 'NONE',  ( 43.01140435219951996, 10.71049967264875491, 29.21067981925357060 ) ) ;
#16704 = VECTOR ( 'NONE', #17921, 1000.000000000000000 ) ;
#16705 = CARTESIAN_POINT ( 'NONE',  ( 48.01140435219951996, 110.3604996726487570, 32.58608133808903773 ) ) ;
#16706 = CARTESIAN_POINT ( 'NONE',  ( 41.64333658814960870, 66.71518717409399812, 38.42115945441014446 ) ) ;
#16707 = CARTESIAN_POINT ( 'NONE',  ( -120.0322075325610598, -136.9891397928655010, -34.99999999999999289 ) ) ;
#16708 = CARTESIAN_POINT ( 'NONE',  ( -143.8425227516148084, -165.0938272943107279, 44.11586579668791330 ) ) ;
#16709 = CARTESIAN_POINT ( 'NONE',  ( 39.92123440845005433, 155.3344580088726161, 29.95742577749336988 ) ) ;
#16710 = CARTESIAN_POINT ( 'NONE',  ( -161.4692556286853176, -178.5630981290893260, 49.65701158161630957 ) ) ;
#16711 = CARTESIAN_POINT ( 'NONE',  ( 43.01140435219951286, 112.4604996726487514, 39.21067981925356349 ) ) ;
#16712 = CARTESIAN_POINT ( 'NONE',  ( 46.10157429594899270, 150.8344580088725593, 38.46393386101376421 ) ) ;
#16713 = CARTESIAN_POINT ( 'NONE',  ( 46.59305225739526435, 127.5797705074273267, 36.81289934271958941 ) ) ;
#16714 = CARTESIAN_POINT ( 'NONE',  ( 73.16288888369128074, 103.5245705370889766, 12.14422718744263285 ) ) ;
#16715 = LINE ( 'NONE', #11023, #9946 ) ;
#16716 = CARTESIAN_POINT ( 'NONE',  ( 47.43856463449118621, 112.6151871740939896, 34.21067981925357060 ) ) ;
#16717 = DIRECTION ( 'NONE',  ( 1.000000000000000000, 0.000000000000000000, 0.000000000000000000 ) ) ;
#16718 = CARTESIAN_POINT ( 'NONE',  ( 41.46631938032478359, 126.3844580088725706, 38.96596240072933170 ) ) ;
#16719 = CARTESIAN_POINT ( 'NONE',  ( 34.72595348466361287, 146.8618156516888291, -3.415175568290148345 ) ) ;
#16720 = CARTESIAN_POINT ( 'NONE',  ( 116.4417310231185780, -126.9891397928655010, 0.3429884183836981459 ) ) ;
#16721 = CARTESIAN_POINT ( 'NONE',  ( 39.42975644700377558, 99.67977050742732104, 36.81289934271958941 ) ) ;
#16722 =( BOUNDED_CURVE ( )  B_SPLINE_CURVE ( 2, ( #16541, #6530, #14891, #4871, #19986, #18541, #10172, #9841, #18319, #3220, #6652, #1568, #15003 ),
 .UNSPECIFIED., .F., .F. ) 
 B_SPLINE_CURVE_WITH_KNOTS ( ( 3, 2, 2, 2, 2, 2, 3 ),
 ( 0.1397058823529411797, 0.1411764705882352922, 0.1441176470588235170, 0.1470588235294117696, 0.1499999999999999944, 0.1529411764705882470, 0.1544117647058823595 ),
 .UNSPECIFIED. ) 
 CURVE ( )  GEOMETRIC_REPRESENTATION_ITEM ( )  RATIONAL_B_SPLINE_CURVE ( ( 0.9755282581475768211, 0.9755282581475768211, 1.000000000000000000, 0.9510565162951535312, 1.000000000000000000, 0.9510565162951535312, 1.000000000000000000, 0.9510565162951535312, 1.000000000000000000, 0.9510565162951535312, 1.000000000000000000, 0.9755282581475768211, 0.9755282581475768211 ) ) 
 REPRESENTATION_ITEM ( '' )  );
#16723 = ORIENTED_EDGE ( 'NONE', *, *, #17447, .T. ) ;
#16724 = CONICAL_SURFACE ( 'NONE', #10059, 9.000000000000007105, 0.7853981633974457255 ) ;
#16725 = CARTESIAN_POINT ( 'NONE',  ( -142.0420953463936087, -195.6584106276440593, 49.65701158161630957 ) ) ;
#16726 = ORIENTED_EDGE ( 'NONE', *, *, #2549, .F. ) ;
#16727 = CARTESIAN_POINT ( 'NONE',  ( 48.01140435219951996, 82.28445800887257633, 34.21067981925357060 ) ) ;
#16728 = FACE_OUTER_BOUND ( 'NONE', #20966, .T. ) ;
#16729 = CARTESIAN_POINT ( 'NONE',  ( 46.10157429594899270, 143.6604996726487400, 29.95742577749337343 ) ) ;
#16731 = CARTESIAN_POINT ( 'NONE',  ( 65.91867393726404600, 103.5983250578868109, 0.3515012976045437387 ) ) ;
#16730 = CARTESIAN_POINT ( 'NONE',  ( 44.37947211624943833, 95.21518717409399812, 30.00020018409699318 ) ) ;
#16732 = EDGE_CURVE ( 'NONE', #11079, #1056, #7875, .T. ) ;
#16733 = CARTESIAN_POINT ( 'NONE',  ( -159.0959885057557983, -169.8584106276440764, 55.19815736654470584 ) ) ;
#16734 = CARTESIAN_POINT ( 'NONE',  ( -142.0420953463936087, -195.3938272943107393, 49.65701158161630957 ) ) ;
#16736 = CYLINDRICAL_SURFACE ( 'NONE', #4099, 27.14138364107347812 ) ;
#16735 = CARTESIAN_POINT ( 'NONE',  ( -159.5594255724347761, -178.8630981290893089, 43.77915905869157598 ) ) ;
#16737 = CARTESIAN_POINT ( 'NONE',  ( -149.8854112254399524, -189.7362167067690280, 59.65701158161632378 ) ) ;
#16738 = FACE_OUTER_BOUND ( 'NONE', #3041, .T. ) ;
#16739 = CARTESIAN_POINT ( 'NONE',  ( 38.96631938032478359, 78.41049967264873999, 31.27175355779120025 ) ) ;
#16740 = CARTESIAN_POINT ( 'NONE',  ( 45.74753988029933538, 155.3297705074273267, 30.44471234641811819 ) ) ;
#16741 = CARTESIAN_POINT ( 'NONE',  ( -120.0322075325610598, -136.9891397928655010, -54.65701158161630246 ) ) ;
#16742 = CARTESIAN_POINT ( 'NONE',  ( 53.71239221804358976, 87.38980250447106357, 6.982120393166105998 ) ) ;
#16743 = CARTESIAN_POINT ( 'NONE',  ( 38.58424406990785371, 140.9651871740939839, 32.77220824515697473 ) ) ;
#16744 = CIRCLE ( 'NONE', #14266, 10.00000000000000888 ) ;
#16745 = CARTESIAN_POINT ( 'NONE',  ( -160.8964159109769696, -164.0438272943107449, 46.59394152635518793 ) ) ;
#16746 = CARTESIAN_POINT ( 'NONE',  ( -154.3824083646099439, -176.7584106276440536, 40.69124936498395328 ) ) ;
#16747 = ORIENTED_EDGE ( 'NONE', *, *, #15515, .T. ) ;
#16748 = CARTESIAN_POINT ( 'NONE',  ( 138.2733499813809885, 177.2661675079481540, -29.99999999999997868 ) ) ;
#16749 = CARTESIAN_POINT ( 'NONE',  ( -159.0959885057557983, -160.8584106276440480, 55.19815736654470584 ) ) ;
#16750 = CARTESIAN_POINT ( 'NONE',  ( 21.96620680132455306, 138.7984961796735490, 1.985398331534963923 ) ) ;
#16751 = DIRECTION ( 'NONE',  ( 1.000000000000000000, 0.000000000000000000, 0.000000000000000000 ) ) ;
#16752 = CARTESIAN_POINT ( 'NONE',  ( 39.42975644700377558, 128.8151871740940067, 31.60846029578754468 ) ) ;
#16753 = ORIENTED_EDGE ( 'NONE', *, *, #8565, .F. ) ;
#16754 = EDGE_LOOP ( 'NONE', ( #4304, #8507, #14274, #8068, #9173 ) ) ;
#16755 = CARTESIAN_POINT ( 'NONE',  ( 38.01140435219952707, 146.9344580088725820, 35.83527830041809636 ) ) ;
#16756 = ORIENTED_EDGE ( 'NONE', *, *, #8065, .F. ) ;
#16757 = CARTESIAN_POINT ( 'NONE',  ( 44.55648932407425633, 108.6844580088725820, 38.96596240072933170 ) ) ;
#16758 = CARTESIAN_POINT ( 'NONE',  ( 45.74753988029934249, 158.3297705074273267, 30.44471234641812174 ) ) ;
#16759 = CIRCLE ( 'NONE', #15702, 9.000000000000007105 ) ;
#16760 = CARTESIAN_POINT ( 'NONE',  ( 46.59305225739526435, 67.57977050742732672, 36.81289934271958941 ) ) ;
#16762 = CARTESIAN_POINT ( 'NONE',  ( 15.38454125381035098, 114.2504036285165654, 1.942219256913226388 ) ) ;
#16761 = CARTESIAN_POINT ( 'NONE',  ( 39.42975644700377558, 126.4151871740940010, 36.81289934271958941 ) ) ;
#16763 = CIRCLE ( 'NONE', #4805, 4.999999999999997335 ) ;
#16764 = EDGE_CURVE ( 'NONE', #9830, #7201, #12348, .T. ) ;
#16765 = CARTESIAN_POINT ( 'NONE',  ( 41.46631938032478359, 78.11049967264874283, 29.45539723777780239 ) ) ;
#16766 = CARTESIAN_POINT ( 'NONE',  ( -151.4692556286852891, -183.2391397928654726, 39.65701158161629536 ) ) ;
#16767 = CARTESIAN_POINT ( 'NONE',  ( 43.01140435219951996, 94.90707761860558378, 29.21067981925357060 ) ) ;
#16768 = CARTESIAN_POINT ( 'NONE',  ( 42.21948215057684450, 138.0373810949690210, 29.21067981925356705 ) ) ;
#16769 = CARTESIAN_POINT ( 'NONE',  ( 44.37947211624943833, 89.21518717409399812, 30.00020018409699318 ) ) ;
#16770 = CARTESIAN_POINT ( 'NONE',  ( 41.46631938032478359, 82.31049967264873146, 38.96596240072933170 ) ) ;
#16771 = PLANE ( 'NONE',  #9576 ) ;
#16772 = ORIENTED_EDGE ( 'NONE', *, *, #3947, .T. ) ;
#16773 = CARTESIAN_POINT ( 'NONE',  ( 43.01140435219951286, 65.62977050742730967, 29.55568802177586463 ) ) ;
#16774 = EDGE_CURVE ( 'NONE', #18306, #16231, #2904, .T. ) ;
#16775 = CARTESIAN_POINT ( 'NONE',  ( -160.8964159109769696, -191.0084106276440821, 52.72008163687743121 ) ) ;
#16776 = AXIS2_PLACEMENT_3D ( 'NONE', #7129, #18479, #13517 ) ;
#16777 = CARTESIAN_POINT ( 'NONE',  ( 74.61827669547474784, 133.2649018527303895, -2.855682626312802785 ) ) ;
#16778 = CARTESIAN_POINT ( 'NONE',  ( -145.6429501568359797, -180.2084106276440707, 41.63779006702063867 ) ) ;
#16779 = ORIENTED_EDGE ( 'NONE', *, *, #14765, .F. ) ;
#16780 = CARTESIAN_POINT ( 'NONE',  ( 46.59305225739526435, 151.9151871740940010, 31.60846029578754468 ) ) ;
#16781 = DIRECTION ( 'NONE',  ( -0.9385982292947087080, -0.3450121214752278620, 1.836742322155470738E-16 ) ) ;
#16782 = CARTESIAN_POINT ( 'NONE',  ( 38.58424406990785371, 111.2297705074273324, 32.77220824515697473 ) ) ;
#16783 = CARTESIAN_POINT ( 'NONE',  ( 68.88151390383544026, 142.3271613368909811, -9.208263745312144977 ) ) ;
#16784 = ORIENTED_EDGE ( 'NONE', *, *, #15853, .F. ) ;
#16785 = EDGE_CURVE ( 'NONE', #14880, #310, #3082, .T. ) ;
#16786 = CARTESIAN_POINT ( 'NONE',  ( 71.13433436327568415, 121.9840874124550965, -8.414894741535439593 ) ) ;
#16787 = EDGE_LOOP ( 'NONE', ( #6401, #10910, #3003, #8226, #2547, #2976, #9990, #8883, #6743, #11934 ) ) ;
#16788 = CARTESIAN_POINT ( 'NONE',  ( 42.21948215057684450, 128.1113394311928175, 29.21067981925356705 ) ) ;
#16789 = CARTESIAN_POINT ( 'NONE',  ( 38.58424406990786082, 159.1151871740940180, 34.21067981925357060 ) ) ;
#16790 = VECTOR ( 'NONE', #2496, 1000.000000000000000 ) ;
#16791 = CARTESIAN_POINT ( 'NONE',  ( 18.35401747797491723, 143.4883766228698221, 10.92869415326320670 ) ) ;
#16792 = DIRECTION ( 'NONE',  ( 0.000000000000000000, 0.000000000000000000, -1.000000000000000000 ) ) ;
#16793 = LINE ( 'NONE', #18567, #1211 ) ;
#16794 = CARTESIAN_POINT ( 'NONE',  ( -143.3790856849358306, -175.2891397928654840, 55.53486410454105027 ) ) ;
#16795 = CARTESIAN_POINT ( 'NONE',  ( 83.67254549292280785, -61.68114226949890622, 30.00000000000000000 ) ) ;
#16796 = CARTESIAN_POINT ( 'NONE',  ( -151.4692556286853176, -193.7391397928655010, 59.65701158161632378 ) ) ;
#16797 = CARTESIAN_POINT ( 'NONE',  ( 38.01140435219952707, 98.63445800887257064, 32.58608133808903773 ) ) ;
#16798 = CARTESIAN_POINT ( 'NONE',  ( 41.64333658814960870, 90.97977050742731819, 38.42115945441014446 ) ) ;
#16799 = CARTESIAN_POINT ( 'NONE',  ( 14.81332417359726783, 119.6334487847019403, -4.843746996953559147 ) ) ;
#16800 = CARTESIAN_POINT ( 'NONE',  ( -154.3824083646099439, -172.2938272943107165, 58.62277379824867296 ) ) ;
#16801 = CARTESIAN_POINT ( 'NONE',  ( 38.58424406990786082, 87.11518717409400381, 34.21067981925357060 ) ) ;
#16802 = VECTOR ( 'NONE', #9170, 1000.000000000000000 ) ;
#16803 = CARTESIAN_POINT ( 'NONE',  ( 43.01140435219951996, 10.71049967264875491, 34.21067981925357060 ) ) ;
#16804 = ORIENTED_EDGE ( 'NONE', *, *, #9259, .F. ) ;
#16805 = CARTESIAN_POINT ( 'NONE',  ( 43.01140435219951996, 10.71049967264875491, 34.21067981925357060 ) ) ;
#16806 = CARTESIAN_POINT ( 'NONE',  ( 9.976645104453018220, 110.9295780357170571, 15.79146183154218619 ) ) ;
#16807 = CARTESIAN_POINT ( 'NONE',  ( 43.01140435219951286, 143.6297705074272812, 29.55568802177586107 ) ) ;
#16808 = CARTESIAN_POINT ( 'NONE',  ( 15.42009695863806229, 114.4785911120537634, -4.053384917639696994 ) ) ;
#16809 = EDGE_CURVE ( 'NONE', #7439, #5452, #7024, .T. ) ;
#16810 = DIRECTION ( 'NONE',  ( -0.3450121214752278065, 0.9385982292947087080, -0.000000000000000000 ) ) ;
#16811 = ORIENTED_EDGE ( 'NONE', *, *, #980, .T. ) ;
#16812 = CARTESIAN_POINT ( 'NONE',  ( 39.42975644700377558, 147.0797705074273267, 31.60846029578754468 ) ) ;
#16813 = CARTESIAN_POINT ( 'NONE',  ( 47.43856463449117200, 94.72977050742733240, 35.64915139335016647 ) ) ;
#16814 = CARTESIAN_POINT ( 'NONE',  ( 38.01140435219952707, 141.8604996726487570, 35.83527830041809636 ) ) ;
#16815 = CARTESIAN_POINT ( 'NONE',  ( 48.01140435219951996, 104.0604996726487457, 35.83527830041810347 ) ) ;
#16816 = CARTESIAN_POINT ( 'NONE',  ( 38.58424406990786082, 60.11518717409400381, 34.21067981925357060 ) ) ;
#16817 = CARTESIAN_POINT ( 'NONE',  ( -151.4692556286852607, -170.3130981290892692, 39.65701158161629536 ) ) ;
#16818 = CARTESIAN_POINT ( 'NONE',  ( -157.2955611005345986, -164.3438272943107279, 41.63779006702063867 ) ) ;
#16819 = CARTESIAN_POINT ( 'NONE',  ( -151.4692556286852891, -126.9891397928655010, 49.65701158161630957 ) ) ;
#16820 = CARTESIAN_POINT ( 'NONE',  ( -148.3790856849358306, -170.4630981290893033, 40.14644641866477315 ) ) ;
#16821 = FACE_OUTER_BOUND ( 'NONE', #3890, .T. ) ;
#16822 = CARTESIAN_POINT ( 'NONE',  ( 39.92123440845004723, 140.3344580088726161, 29.95742577749337343 ) ) ;
#16823 = CARTESIAN_POINT ( 'NONE',  ( 38.58424406990784661, 123.5297705074273438, 35.64915139335016647 ) ) ;
#16824 = CARTESIAN_POINT ( 'NONE',  ( 11.87357267856223864, 134.3244722033052767, 8.572888645784400907 ) ) ;
#16825 = CARTESIAN_POINT ( 'NONE',  ( 47.05648932407426344, 99.98445800887257917, 37.14960608071593384 ) ) ;
#16826 = CARTESIAN_POINT ( 'NONE',  ( 44.37947211624943833, 116.2151871740940123, 30.00020018409699318 ) ) ;
#16827 = LINE ( 'NONE', #20051, #7612 ) ;
#16828 = FACE_OUTER_BOUND ( 'NONE', #15437, .T. ) ;
#16829 = CARTESIAN_POINT ( 'NONE',  ( 76.55129369653414528, 113.4641082036936837, -0.2041528983002713349 ) ) ;
#16830 = ADVANCED_FACE ( 'NONE', ( #17555 ), #813, .T. ) ;
#16831 = CARTESIAN_POINT ( 'NONE',  ( 26.65597624659334031, 142.8797025615743337, -3.772066457372480475 ) ) ;
#16832 = CARTESIAN_POINT ( 'NONE',  ( -143.3790856849358306, -186.3630981290893089, 55.53486410454105027 ) ) ;
#16833 = CARTESIAN_POINT ( 'NONE',  ( 45.74753988029934249, 83.32977050742732672, 30.44471234641812174 ) ) ;
#16834 = VERTEX_POINT ( 'NONE', #14362 ) ;
#16835 = FACE_BOUND ( 'NONE', #20765, .T. ) ;
#16836 = ORIENTED_EDGE ( 'NONE', *, *, #3797, .F. ) ;
#16837 = CARTESIAN_POINT ( 'NONE',  ( 38.96631938032478359, 72.08445800887257349, 37.14960608071593384 ) ) ;
#16838 = CARTESIAN_POINT ( 'NONE',  ( 43.01140435219951996, 10.71049967264875491, 39.21067981925356349 ) ) ;
#16839 = CARTESIAN_POINT ( 'NONE',  ( 48.01140435219951996, 137.2104996726487514, 34.21067981925357060 ) ) ;
#16841 = CARTESIAN_POINT ( 'NONE',  ( 76.02541712503827398, 128.6535784478189726, -7.704039830276845358 ) ) ;
#16840 = CARTESIAN_POINT ( 'NONE',  ( 44.37947211624943833, 89.21518717409399812, 30.00020018409699318 ) ) ;
#16842 = CARTESIAN_POINT ( 'NONE',  ( -145.6429501568359797, -157.1084106276440480, 57.67623309621198047 ) ) ;
#16843 = CARTESIAN_POINT ( 'NONE',  ( -151.4692556286852891, -190.1438272943107393, 59.56931450028537256 ) ) ;
#16844 = CARTESIAN_POINT ( 'NONE',  ( 38.01140435219952707, 93.71049967264875136, 34.21067981925357060 ) ) ;
#16845 = CARTESIAN_POINT ( 'NONE',  ( 43.80332655382220253, 80.88361825032846752, 29.21067981925356705 ) ) ;
#16846 = CARTESIAN_POINT ( 'NONE',  ( 44.37947211624943833, 151.2797705074273438, 38.42115945441014446 ) ) ;
#16847 = DIRECTION ( 'NONE',  ( 0.3450121214752279175, -0.9385982292947087080, -0.000000000000000000 ) ) ;
#16848 = CARTESIAN_POINT ( 'NONE',  ( 69.27296957579615366, 97.94681810169329594, -0.6368323762655749842 ) ) ;
#16849 = CARTESIAN_POINT ( 'NONE',  ( 38.58424406990786082, 147.1151871740939896, 34.21067981925357060 ) ) ;
#16850 = CARTESIAN_POINT ( 'NONE',  ( -143.8425227516148084, -159.0938272943107279, 44.11586579668791330 ) ) ;
#16851 = CARTESIAN_POINT ( 'NONE',  ( -154.3824083646099439, -170.7584106276440536, 40.69124936498395328 ) ) ;
#16852 = ORIENTED_EDGE ( 'NONE', *, *, #10434, .T. ) ;
#16853 = CARTESIAN_POINT ( 'NONE',  ( 45.74753988029934249, 61.16518717409399386, 37.97664729208901235 ) ) ;
#16854 =( BOUNDED_CURVE ( )  B_SPLINE_CURVE ( 2, ( #2238, #15888, #3682, #17541, #801, #14238, #5331, #17331, #10410, #17112, #7214, #2028, #5431 ),
 .UNSPECIFIED., .F., .F. ) 
 B_SPLINE_CURVE_WITH_KNOTS ( ( 3, 2, 2, 2, 2, 2, 3 ),
 ( 0.3897058823529411797, 0.3911764705882352922, 0.3941176470588235170, 0.3970588235294117418, 0.4000000000000000222, 0.4029411764705882470, 0.4044117647058823595 ),
 .UNSPECIFIED. ) 
 CURVE ( )  GEOMETRIC_REPRESENTATION_ITEM ( )  RATIONAL_B_SPLINE_CURVE ( ( 0.9755282581475768211, 0.9755282581475768211, 1.000000000000000000, 0.9510565162951535312, 1.000000000000000000, 0.9510565162951535312, 1.000000000000000000, 0.9510565162951535312, 1.000000000000000000, 0.9510565162951535312, 1.000000000000000000, 0.9755282581475768211, 0.9755282581475768211 ) ) 
 REPRESENTATION_ITEM ( '' )  );
#16855 = CARTESIAN_POINT ( 'NONE',  ( -145.6429501568359797, -163.1084106276440195, 57.67623309621198047 ) ) ;
#16856 = CARTESIAN_POINT ( 'NONE',  ( 27.23529593042425390, 96.43589704216468306, 0.08059930645588880838 ) ) ;
#16857 = CARTESIAN_POINT ( 'NONE',  ( 39.92123440845005433, 135.2344580088725365, 38.46393386101375711 ) ) ;
#16858 = CARTESIAN_POINT ( 'NONE',  ( 39.42975644700377558, 123.4151871740940010, 36.81289934271958941 ) ) ;
#16859 = EDGE_LOOP ( 'NONE', ( #1143, #15468, #10937, #19409, #6640 ) ) ;
#16860 = ORIENTED_EDGE ( 'NONE', *, *, #5917, .T. ) ;
#16861 = CARTESIAN_POINT ( 'NONE',  ( -151.4692556286852607, -192.2391397928655010, 39.65701158161629536 ) ) ;
#16862 = ORIENTED_EDGE ( 'NONE', *, *, #6638, .F. ) ;
#16863 = CARTESIAN_POINT ( 'NONE',  ( 44.55648932407425633, 100.8844580088725849, 29.45539723777780239 ) ) ;
#16864 = CIRCLE ( 'NONE', #14047, 9.000000000000007105 ) ;
#16865 = CARTESIAN_POINT ( 'NONE',  ( 46.59305225739526435, 157.5797705074273267, 36.81289934271958941 ) ) ;
#16866 = VECTOR ( 'NONE', #19805, 1000.000000000000114 ) ;
#16867 = CARTESIAN_POINT ( 'NONE',  ( 41.64333658814960870, 63.97977050742731109, 38.42115945441014446 ) ) ;
#16869 = CARTESIAN_POINT ( 'NONE',  ( 26.83015598135647295, 142.9878415585355071, 17.22988066553158149 ) ) ;
#16868 = CARTESIAN_POINT ( 'NONE',  ( 47.43856463449118621, 130.6151871740940180, 34.21067981925357060 ) ) ;
#16870 = CARTESIAN_POINT ( 'NONE',  ( 47.05648932407426344, 85.91049967264873999, 37.14960608071593384 ) ) ;
#16871 = LINE ( 'NONE', #15002, #4773 ) ;
#16872 = CARTESIAN_POINT ( 'NONE',  ( -148.3790856849358306, -171.6630981290893203, 59.16757674456786020 ) ) ;
#16873 = CARTESIAN_POINT ( 'NONE',  ( -155.5590455049452316, -156.0406172220664303, 40.47124262348441448 ) ) ;
#16874 = CARTESIAN_POINT ( 'NONE',  ( 43.01140435219951286, 80.36518717409398960, 29.55568802177586463 ) ) ;
#16875 = CARTESIAN_POINT ( 'NONE',  ( 43.01140435219951286, 80.96049967264873715, 29.21067981925356705 ) ) ;
#16876 = FACE_OUTER_BOUND ( 'NONE', #3210, .T. ) ;
#16877 = EDGE_CURVE ( 'NONE', #6932, #5516, #21104, .T. ) ;
#16878 = ORIENTED_EDGE ( 'NONE', *, *, #1668, .T. ) ;
#16879 = CARTESIAN_POINT ( 'NONE',  ( 41.64333658814960870, 65.77977050742732956, 30.00020018409699318 ) ) ;
#16880 = CARTESIAN_POINT ( 'NONE',  ( -160.8964159109769696, -182.3084106276440650, 46.59394152635518793 ) ) ;
#16881 = CARTESIAN_POINT ( 'NONE',  ( 23.00888394656308122, 147.7027690514567837, -4.855972970016076751 ) ) ;
#16882 = CARTESIAN_POINT ( 'NONE',  ( -157.2955611005346270, -178.7084106276440139, 57.67623309621198047 ) ) ;
#16883 = VERTEX_POINT ( 'NONE', #2463 ) ;
#16884 = CARTESIAN_POINT ( 'NONE',  ( 46.59305225739526435, 148.9151871740940294, 31.60846029578754468 ) ) ;
#16885 = ADVANCED_FACE ( 'NONE', ( #5986 ), #20992, .F. ) ;
#16886 = FACE_OUTER_BOUND ( 'NONE', #21096, .T. ) ;
#16887 = EDGE_CURVE ( 'NONE', #1525, #4150, #11823, .T. ) ;
#16888 = CARTESIAN_POINT ( 'NONE',  ( 46.59305225739526435, 119.1797705074273068, 31.60846029578754468 ) ) ;
#16889 = CARTESIAN_POINT ( 'NONE',  ( 75.80354157443048280, 110.0810758630161672, 5.910575721798123183 ) ) ;
#16890 = EDGE_LOOP ( 'NONE', ( #899, #20995, #7824, #11141 ) ) ;
#16891 = CARTESIAN_POINT ( 'NONE',  ( 34.17400395940548918, 146.6865494356538875, -10.43883331896520694 ) ) ;
#16892 = ORIENTED_EDGE ( 'NONE', *, *, #13309, .T. ) ;
#16893 = CARTESIAN_POINT ( 'NONE',  ( 46.59305225739526435, 110.1797705074273210, 31.60846029578754468 ) ) ;
#16894 = EDGE_CURVE ( 'NONE', #5724, #16672, #11381, .T. ) ;
#16895 = LINE ( 'NONE', #13590, #8692 ) ;
#16896 = CARTESIAN_POINT ( 'NONE',  ( 47.43856463449117200, 154.4651871740940123, 35.64915139335016647 ) ) ;
#16897 = CARTESIAN_POINT ( 'NONE',  ( 16.50170782505827560, 141.4403336307199197, 3.843654360456687513 ) ) ;
#16898 = CLOSED_SHELL ( 'NONE', ( #20263, #19897, #2903, #7076, #18687, #18101, #14664, #21046, #16056, #12425, #16397 ) ) ;
#16899 = FACE_OUTER_BOUND ( 'NONE', #4658, .T. ) ;
#16900 = CARTESIAN_POINT ( 'NONE',  ( 43.01140435219951286, 80.96049967264873715, 29.21067981925356705 ) ) ;
#16901 = CARTESIAN_POINT ( 'NONE',  ( -141.4692556286852891, -184.1391397928654783, 52.90620854394536821 ) ) ;
#16902 = CARTESIAN_POINT ( 'NONE',  ( 43.80332655382220253, 101.8836182503284675, 29.21067981925356705 ) ) ;
#16903 = LINE ( 'NONE', #8550, #12516 ) ;
#16904 = CARTESIAN_POINT ( 'NONE',  ( 47.05648932407426344, 91.91049967264873999, 37.14960608071593384 ) ) ;
#16905 = LINE ( 'NONE', #10415, #9247 ) ;
#16906 = EDGE_CURVE ( 'NONE', #21813, #16694, #2876, .T. ) ;
#16907 = CARTESIAN_POINT ( 'NONE',  ( 41.64333658814960870, 96.97977050742731819, 38.42115945441014446 ) ) ;
#16908 = CARTESIAN_POINT ( 'NONE',  ( 60.38095089740433252, 142.1228462996803046, -2.343495028824083004 ) ) ;
#16909 = CARTESIAN_POINT ( 'NONE',  ( -148.5561028927606344, -171.9938272943107336, 58.62277379824867296 ) ) ;
#16910 = CARTESIAN_POINT ( 'NONE',  ( 40.27526882409969744, 80.66518717409400097, 30.44471234641812174 ) ) ;
#16911 = CARTESIAN_POINT ( 'NONE',  ( -151.4692556286852891, -195.2391397928655010, 39.65701158161629536 ) ) ;
#16912 = ORIENTED_EDGE ( 'NONE', *, *, #7465, .T. ) ;
#16913 = CARTESIAN_POINT ( 'NONE',  ( 91.17254549292282206, -61.68114226949890622, -46.21320343559645494 ) ) ;
#16914 = EDGE_CURVE ( 'NONE', #15661, #2045, #11710, .T. ) ;
#16915 = CARTESIAN_POINT ( 'NONE',  ( 42.21854335081802390, 85.68333463812091111, 14.36287948008016890 ) ) ;
#16916 = CARTESIAN_POINT ( 'NONE',  ( 57.63517438308760177, 95.88943085326536675, -6.196329169593343345 ) ) ;
#16917 = MECHANICAL_DESIGN_GEOMETRIC_PRESENTATION_REPRESENTATION (  '', ( #14803 ), #14095 ) ;
#16918 = CARTESIAN_POINT ( 'NONE',  ( 41.46631938032478359, 120.3844580088725849, 38.96596240072933170 ) ) ;
#16919 = EDGE_LOOP ( 'NONE', ( #7234, #12925, #17289, #10693 ) ) ;
#16920 = CARTESIAN_POINT ( 'NONE',  ( 38.58424406990786082, 147.3797705074273097, 34.21067981925357060 ) ) ;
#16921 = CARTESIAN_POINT ( 'NONE',  ( 41.64333658814960870, 96.97977050742731819, 38.42115945441014446 ) ) ;
#16922 = DIRECTION ( 'NONE',  ( 0.000000000000000000, 0.000000000000000000, 1.000000000000000000 ) ) ;
#16923 = CARTESIAN_POINT ( 'NONE',  ( -39.76538861119684753, -7.722638610254815461, 4.000000000000021316 ) ) ;
#16924 = DIRECTION ( 'NONE',  ( 0.000000000000000000, 0.000000000000000000, 1.000000000000000000 ) ) ;
#16925 = CARTESIAN_POINT ( 'NONE',  ( 43.01140435219951996, 10.71049967264875491, 29.21067981925357060 ) ) ;
#16926 = CARTESIAN_POINT ( 'NONE',  ( -120.0322075325610740, -136.9891397928655010, 49.65701158161630957 ) ) ;
#16927 = CARTESIAN_POINT ( 'NONE',  ( -161.4692556286852607, -166.7130981290893317, 46.40781461928724383 ) ) ;
#16928 = CARTESIAN_POINT ( 'NONE',  ( 41.46631938032478359, 140.1844580088725820, 29.45539723777780239 ) ) ;
#16929 = CARTESIAN_POINT ( 'NONE',  ( 44.37947211624943833, 121.2797705074273296, 38.42115945441014446 ) ) ;
#16930 = CARTESIAN_POINT ( 'NONE',  ( 66.11232864078046134, 136.2219195394164899, -3.014685448219384334 ) ) ;
#16931 = CARTESIAN_POINT ( 'NONE',  ( 47.05648932407426344, 100.5844580088725877, 31.27175355779120025 ) ) ;
#16932 = CARTESIAN_POINT ( 'NONE',  ( 45.74753988029934249, 118.1651871740939868, 37.97664729208901235 ) ) ;
#16933 = DIRECTION ( 'NONE',  ( 1.000000000000000000, 0.000000000000000000, 0.000000000000000000 ) ) ;
#16934 = CARTESIAN_POINT ( 'NONE',  ( 73.74613032677598312, 134.8023270448005064, -0.9181577650121128809 ) ) ;
#16935 = CARTESIAN_POINT ( 'NONE',  ( 70.85748824340309682, 124.3570181999574515, -1.510321027129504889 ) ) ;
#16936 = LINE ( 'NONE', #18387, #6164 ) ;
#16937 = CARTESIAN_POINT ( 'NONE',  ( 45.74753988029934249, 85.42977050742730682, 37.97664729208901235 ) ) ;
#16938 = VERTEX_POINT ( 'NONE', #16338 ) ;
#16939 = DIRECTION ( 'NONE',  ( -0.000000000000000000, -1.000000000000000000, -0.000000000000000000 ) ) ;
#16940 = CARTESIAN_POINT ( 'NONE',  ( 48.01140435219951996, 70.43445800887258201, 32.58608133808903773 ) ) ;
#16941 = PLANE ( 'NONE',  #14396 ) ;
#16942 = CARTESIAN_POINT ( 'NONE',  ( 46.10157429594899270, 130.7604996726487343, 38.46393386101376421 ) ) ;
#16944 = CARTESIAN_POINT ( 'NONE',  ( 63.68221904981356829, 147.0951523173380338, -15.44234037292825690 ) ) ;
#16943 = CARTESIAN_POINT ( 'NONE',  ( 39.42975644700377558, 86.81518717409400665, 31.60846029578754468 ) ) ;
#16945 = CARTESIAN_POINT ( 'NONE',  ( -160.8964159109769696, -161.3084106276440082, 46.59394152635518793 ) ) ;
#16946 = EDGE_CURVE ( 'NONE', #5629, #12140, #13265, .T. ) ;
#16947 = CARTESIAN_POINT ( 'NONE',  ( -145.6429501568359797, -179.9438272943107506, 41.63779006702063867 ) ) ;
#16948 = CARTESIAN_POINT ( 'NONE',  ( 42.21948215057687293, 94.38361825032848174, 39.21067981925357060 ) ) ;
#16949 = CARTESIAN_POINT ( 'NONE',  ( -145.2889157411863721, -194.6130981290892805, 41.15050349809590102 ) ) ;
#16950 = VECTOR ( 'NONE', #4113, 1000.000000000000000 ) ;
#16951 = EDGE_CURVE ( 'NONE', #11189, #13667, #14688, .T. ) ;
#16952 = VECTOR ( 'NONE', #7770, 1000.000000000000227 ) ;
#16953 = CARTESIAN_POINT ( 'NONE',  ( 48.01140435219951996, 68.21049967264873715, 34.21067981925357060 ) ) ;
#16954 = DIRECTION ( 'NONE',  ( -1.233581138472395521E-15, 0.000000000000000000, 1.000000000000000000 ) ) ;
#16955 = CARTESIAN_POINT ( 'NONE',  ( 45.74753988029933538, 148.4297705074273210, 37.97664729208901946 ) ) ;
#16956 = CARTESIAN_POINT ( 'NONE',  ( 46.10157429594899270, 157.7604996726487343, 38.46393386101375711 ) ) ;
#16957 = CARTESIAN_POINT ( 'NONE',  ( 68.29446192123552350, 96.82662215664792882, 13.41040346623746515 ) ) ;
#16958 = CARTESIAN_POINT ( 'NONE',  ( 40.27526882409969744, 144.5651871740940067, 37.97664729208901235 ) ) ;
#16959 = LINE ( 'NONE', #13658, #509 ) ;
#16960 = CARTESIAN_POINT ( 'NONE',  ( -143.8425227516148084, -177.3584106276440480, 44.11586579668791330 ) ) ;
#16961 = CARTESIAN_POINT ( 'NONE',  ( 38.96631938032478359, 78.08445800887257349, 37.14960608071593384 ) ) ;
#16962 = CARTESIAN_POINT ( 'NONE',  ( -145.6429501568359797, -160.1084106276440480, 57.67623309621198047 ) ) ;
#16963 = CARTESIAN_POINT ( 'NONE',  ( 16.02160000510927418, 128.3529272436884128, 1.509170735004851549 ) ) ;
#16964 = CARTESIAN_POINT ( 'NONE',  ( 43.01140435219951996, 119.9070776186055838, -19.99999999999997868 ) ) ;
#16965 = CARTESIAN_POINT ( 'NONE',  ( 40.27526882409969033, 125.6651871740939868, 30.44471234641811819 ) ) ;
#16966 = EDGE_LOOP ( 'NONE', ( #3179, #19228, #2145, #9288 ) ) ;
#16967 = EDGE_CURVE ( 'NONE', #17262, #10554, #7983, .T. ) ;
#16968 = ORIENTED_EDGE ( 'NONE', *, *, #16967, .F. ) ;
#16969 = CARTESIAN_POINT ( 'NONE',  ( 43.01140435219951286, 114.5344580088725621, 39.21067981925356349 ) ) ;
#16970 = ORIENTED_EDGE ( 'NONE', *, *, #19571, .T. ) ;
#16971 = CARTESIAN_POINT ( 'NONE',  ( 46.10157429594899270, 103.7344580088725934, 29.95742577749337343 ) ) ;
#16972 = CARTESIAN_POINT ( 'NONE',  ( 38.58424406990786082, 159.1151871740940180, 34.21067981925357060 ) ) ;
#16973 = CARTESIAN_POINT ( 'NONE',  ( 38.01140435219951996, 159.5604996726487457, 32.58608133808903773 ) ) ;
#16975 = CARTESIAN_POINT ( 'NONE',  ( 69.30627838890079317, 109.9422389716749535, -13.93421298911417416 ) ) ;
#16974 = CARTESIAN_POINT ( 'NONE',  ( 38.58424406990786082, 120.1151871740940038, 34.21067981925357060 ) ) ;
#16976 = CARTESIAN_POINT ( 'NONE',  ( 38.01140435219951996, 81.86049967264874283, 35.83527830041810347 ) ) ;
#16977 = CARTESIAN_POINT ( 'NONE',  ( 47.05648932407426344, 147.9844580088725934, 37.14960608071593384 ) ) ;
#16978 = FACE_OUTER_BOUND ( 'NONE', #7337, .T. ) ;
#16979 = CARTESIAN_POINT ( 'NONE',  ( -153.0531000319306543, -191.2362167067690280, 39.65701158161628825 ) ) ;
#16980 =( BOUNDED_CURVE ( )  B_SPLINE_CURVE ( 2, ( #15653, #16979, #14106, #5204, #18649, #3551, #1889, #7837, #16300, #17518, #2429, #11231, #14539 ),
 .UNSPECIFIED., .F., .T. ) 
 B_SPLINE_CURVE_WITH_KNOTS ( ( 3, 2, 2, 2, 2, 2, 3 ),
 ( 0.08928571428571425994, 0.09285714285714286031, 0.1000000000000000056, 0.1071428571428571369, 0.1142857142857142821, 0.1214285714285714274, 0.1249999999999999584 ),
 .UNSPECIFIED. ) 
 CURVE ( )  GEOMETRIC_REPRESENTATION_ITEM ( )  RATIONAL_B_SPLINE_CURVE ( ( 0.9755282581475768211, 0.9755282581475765991, 1.000000000000000000, 0.9510565162951535312, 1.000000000000000000, 0.9510565162951535312, 1.000000000000000000, 0.9510565162951535312, 1.000000000000000000, 0.9510565162951535312, 1.000000000000000000, 0.9755282581475770431, 0.9755282581475768211 ) ) 
 REPRESENTATION_ITEM ( '' )  );
#16981 = CARTESIAN_POINT ( 'NONE',  ( 38.58424406990784661, 75.26518717409399528, 35.64915139335016647 ) ) ;
#16982 = PRODUCT_DEFINITION_CONTEXT ( 'detailed design', #15053, 'design' ) ;
#16983 = CARTESIAN_POINT ( 'NONE',  ( 39.24503612293847254, 144.6228301878137188, 37.51526355657936307 ) ) ;
#16984 = CARTESIAN_POINT ( 'NONE',  ( 43.01140435219951286, 123.5344580088725621, 39.46799094044489209 ) ) ;
#16985 = CARTESIAN_POINT ( 'NONE',  ( 130.1509106190733007, 127.1041540266590602, 4.000000000000003553 ) ) ;
#16986 = ADVANCED_FACE ( 'NONE', ( #18217 ), #3011, .F. ) ;
#16987 = VERTEX_POINT ( 'NONE', #3123 ) ;
#16988 = CARTESIAN_POINT ( 'NONE',  ( -148.5561028927606344, -190.2584106276440536, 58.62277379824867296 ) ) ;
#16989 = CARTESIAN_POINT ( 'NONE',  ( 71.08298874133512868, 139.6419663798271529, -3.093729572736475752 ) ) ;
#16990 = CARTESIAN_POINT ( 'NONE',  ( -160.8964159109769696, -173.1584106276440593, 49.65701158161630957 ) ) ;
#16991 = ORIENTED_EDGE ( 'NONE', *, *, #18540, .F. ) ;
#16992 = CARTESIAN_POINT ( 'NONE',  ( 40.27526882409969033, 153.5651871740940067, 37.97664729208901946 ) ) ;
#16993 = LINE ( 'NONE', #2119, #14476 ) ;
#16994 = CARTESIAN_POINT ( 'NONE',  ( 66.24914683137549787, 94.76885710642066840, 6.506024766557033878 ) ) ;
#16995 = VERTEX_POINT ( 'NONE', #1692 ) ;
#16996 = PRODUCT_RELATED_PRODUCT_CATEGORY ( 'part', '', ( #13296 ) ) ;
#16997 = VERTEX_POINT ( 'NONE', #8422 ) ;
#16998 = CARTESIAN_POINT ( 'NONE',  ( 47.43856463449117200, 113.0297705074273011, 32.77220824515698183 ) ) ;
#16999 = FACE_OUTER_BOUND ( 'NONE', #4332, .T. ) ;
#17000 = FACE_OUTER_BOUND ( 'NONE', #18848, .T. ) ;
#17001 = EDGE_CURVE ( 'NONE', #12307, #120, #20000, .T. ) ;
#17002 = CARTESIAN_POINT ( 'NONE',  ( 38.58424406990784661, 147.2651871740939669, 35.64915139335016647 ) ) ;
#17003 = EDGE_CURVE ( 'NONE', #4221, #1853, #15542, .T. ) ;
#17004 = CARTESIAN_POINT ( 'NONE',  ( 26.90790578767411390, 150.1165885900122987, 3.291480155758420345 ) ) ;
#17005 = LINE ( 'NONE', #18566, #10651 ) ;
#17006 = PLANE ( 'NONE',  #21200 ) ;
#17007 = CARTESIAN_POINT ( 'NONE',  ( -141.4692556286852891, -180.8391397928654669, 46.40781461928724383 ) ) ;
#17008 = ADVANCED_FACE ( 'NONE', ( #1247 ), #19768, .F. ) ;
#17009 = CYLINDRICAL_SURFACE ( 'NONE', #21399, 4.999999999999997335 ) ;
#17010 = CYLINDRICAL_SURFACE ( 'NONE', #19222, 5.000000000000004441 ) ;
#17011 = DIRECTION ( 'NONE',  ( 1.000000000000000000, 0.000000000000000000, -0.000000000000000000 ) ) ;
#17012 = CARTESIAN_POINT ( 'NONE',  ( 43.01140435219951996, 2.710499672648754466, 9.210679819253577705 ) ) ;
#17013 = CARTESIAN_POINT ( 'NONE',  ( 40.27526882409969033, 96.82977050742731251, 37.97664729208901946 ) ) ;
#17014 = CARTESIAN_POINT ( 'NONE',  ( 27.10205971394288582, 96.62443569844734270, -5.915007788698968483 ) ) ;
#17015 = CARTESIAN_POINT ( 'NONE',  ( -160.8964159109769696, -173.0438272943107449, 46.59394152635518793 ) ) ;
#17016 = CARTESIAN_POINT ( 'NONE',  ( 39.42975644700377558, 75.41518717409400097, 36.81289934271958941 ) ) ;
#17017 = CARTESIAN_POINT ( 'NONE',  ( 131.0765927465021434, 198.5836349573982886, 34.00000000000001421 ) ) ;
#17018 = CYLINDRICAL_SURFACE ( 'NONE', #560, 4.999999999999997335 ) ;
#17019 = ORIENTED_EDGE ( 'NONE', *, *, #121, .F. ) ;
#17020 = DIRECTION ( 'NONE',  ( 1.000000000000000000, 0.000000000000000000, -1.915514545828640458E-16 ) ) ;
#17021 = CARTESIAN_POINT ( 'NONE',  ( 46.10157429594899270, 121.7604996726487343, 38.46393386101375711 ) ) ;
#17022 = CARTESIAN_POINT ( 'NONE',  ( 45.76500403897348690, 91.92250713676531859, 1.303787141088997181 ) ) ;
#17023 = EDGE_LOOP ( 'NONE', ( #149, #10344, #20459, #3861, #2488, #6261, #8400 ) ) ;
#17024 = DIRECTION ( 'NONE',  ( 0.9385982292947088190, 0.3450121214752274179, -1.836742322155470491E-16 ) ) ;
#17025 = ORIENTED_EDGE ( 'NONE', *, *, #19413, .F. ) ;
#17026 = CARTESIAN_POINT ( 'NONE',  ( 43.01140435219951286, 137.6297705074273381, 29.55568802177586463 ) ) ;
#17027 = AXIS2_PLACEMENT_3D ( 'NONE', #2701, #9331, #1055 ) ;
#17028 = CARTESIAN_POINT ( 'NONE',  ( 38.58424406990786082, 99.37977050742732388, 34.21067981925357060 ) ) ;
#17029 = CARTESIAN_POINT ( 'NONE',  ( 46.10157429594899270, 151.7604996726487059, 38.46393386101375711 ) ) ;
#17030 = LINE ( 'NONE', #1838, #7291 ) ;
#17031 = FACE_BOUND ( 'NONE', #20941, .T. ) ;
#17032 = AXIS2_PLACEMENT_3D ( 'NONE', #13442, #8381, #6837 ) ;
#17033 = CARTESIAN_POINT ( 'NONE',  ( 41.46631938032478359, 154.3104996726487457, 38.96596240072933170 ) ) ;
#17034 = DIRECTION ( 'NONE',  ( -0.3428981916074316239, 0.9393725726208708160, 0.000000000000000000 ) ) ;
#17035 = CARTESIAN_POINT ( 'NONE',  ( -148.3790856849358306, -164.4630981290893317, 40.14644641866477315 ) ) ;
#17036 = DIRECTION ( 'NONE',  ( 0.000000000000000000, 0.000000000000000000, 1.000000000000000000 ) ) ;
#17037 = CARTESIAN_POINT ( 'NONE',  ( 39.92123440845004723, 144.2344580088725934, 38.46393386101376421 ) ) ;
#17038 = CARTESIAN_POINT ( 'NONE',  ( 44.37947211624943833, 125.4797705074273182, 30.00020018409699318 ) ) ;
#17039 = CARTESIAN_POINT ( 'NONE',  ( 70.07576047146775977, 128.1116393178318731, -2.657569147260473663 ) ) ;
#17040 = DIRECTION ( 'NONE',  ( -0.4999508154438193630, 0.000000000000000000, 0.8660537986390106635 ) ) ;
#17041 = CARTESIAN_POINT ( 'NONE',  ( 38.58424406990785371, 104.9651871740940123, 32.77220824515697473 ) ) ;
#17042 = DIRECTION ( 'NONE',  ( -0.8654262854811262118, 0.000000000000000000, 0.5010362705417048534 ) ) ;
#17043 = CARTESIAN_POINT ( 'NONE',  ( 40.73010619540765020, 85.74955863377461185, -6.589596535617429751 ) ) ;
#17044 = CARTESIAN_POINT ( 'NONE',  ( 68.03731475862628031, 132.9047928164914367, -1.867435455408581912 ) ) ;
#17045 = CARTESIAN_POINT ( 'NONE',  ( -141.4692556286852891, -186.0630981290892976, 49.65701158161630957 ) ) ;
#17046 = CARTESIAN_POINT ( 'NONE',  ( 46.59305225739526435, 82.57977050742731251, 36.81289934271958941 ) ) ;
#17047 = AXIS2_PLACEMENT_3D ( 'NONE', #14188, #2725, #20927 ) ;
#17048 = VERTEX_POINT ( 'NONE', #9749 ) ;
#17049 = EDGE_CURVE ( 'NONE', #15871, #9910, #1359, .T. ) ;
#17050 = CARTESIAN_POINT ( 'NONE',  ( 44.55648932407425633, 110.8104996726487457, 29.45539723777780239 ) ) ;
#17051 = CARTESIAN_POINT ( 'NONE',  ( 39.92123440845004723, 77.33445800887257349, 29.95742577749337343 ) ) ;
#17052 = CARTESIAN_POINT ( 'NONE',  ( 42.21948215057684450, 86.11133943119284595, 29.21067981925356705 ) ) ;
#17053 = CARTESIAN_POINT ( 'NONE',  ( 47.05648932407426344, 128.5104996726487343, 31.27175355779120025 ) ) ;
#17055 = CARTESIAN_POINT ( 'NONE',  ( 64.23777839346797691, 146.6638261710672566, -8.418409733082999225 ) ) ;
#17054 = CARTESIAN_POINT ( 'NONE',  ( 40.27526882409969033, 89.66518717409400097, 30.44471234641811819 ) ) ;
#17056 = CARTESIAN_POINT ( 'NONE',  ( -142.0420953463935803, -159.8084106276440934, 52.72008163687743831 ) ) ;
#17057 = CARTESIAN_POINT ( 'NONE',  ( -148.5561028927606344, -183.9938272943107336, 58.62277379824867296 ) ) ;
#17058 = CARTESIAN_POINT ( 'NONE',  ( -145.2889157411863437, -178.4391397928654044, 58.16351966513671812 ) ) ;
#17059 = CARTESIAN_POINT ( 'NONE',  ( -161.4692556286852607, -193.7130981290893317, 46.40781461928724383 ) ) ;
#17060 = CARTESIAN_POINT ( 'NONE',  ( -151.4692556286853176, -163.7391397928654726, 59.65701158161632378 ) ) ;
#17061 = CARTESIAN_POINT ( 'NONE',  ( -154.5594255724347761, -172.8891397928654783, 59.16757674456785310 ) ) ;
#17062 = CARTESIAN_POINT ( 'NONE',  ( 40.27526882409969033, 150.8297705074273267, 37.97664729208901946 ) ) ;
#17063 = CARTESIAN_POINT ( 'NONE',  ( 45.74753988029933538, 103.4297705074273210, 37.97664729208901946 ) ) ;
#17064 = CARTESIAN_POINT ( 'NONE',  ( 8.829984022807513711, 121.7968051057545580, 16.14860047415989541 ) ) ;
#17065 = CARTESIAN_POINT ( 'NONE',  ( 38.58424406990785371, 132.2651871740939953, 35.64915139335015937 ) ) ;
#17066 = CARTESIAN_POINT ( 'NONE',  ( -161.4692556286852891, -188.6391397928654783, 46.40781461928724383 ) ) ;
#17067 = CARTESIAN_POINT ( 'NONE',  ( -154.3824083646099439, -175.5584106276440366, 58.62277379824867296 ) ) ;
#17068 = CARTESIAN_POINT ( 'NONE',  ( 46.59305225739526435, 64.31518717409399244, 36.81289934271958941 ) ) ;
#17069 = CARTESIAN_POINT ( 'NONE',  ( 71.28213884770818254, 119.1643779896719764, -2.300315981272657240 ) ) ;
#17070 = AXIS2_PLACEMENT_3D ( 'NONE', #7455, #10758, #5782 ) ;
#17071 = DIRECTION ( 'NONE',  ( 0.000000000000000000, 0.000000000000000000, 1.000000000000000000 ) ) ;
#17072 = CARTESIAN_POINT ( 'NONE',  ( 43.01140435219951286, 111.8651871740939896, 38.86567161673127657 ) ) ;
#17073 = VERTEX_POINT ( 'NONE', #1470 ) ;
#17074 = ORIENTED_EDGE ( 'NONE', *, *, #9086, .F. ) ;
#17075 = EDGE_CURVE ( 'NONE', #12683, #19403, #21651, .T. ) ;
#17076 = DIRECTION ( 'NONE',  ( -1.000000000000000000, -2.779543948608941985E-16, 0.000000000000000000 ) ) ;
#17077 = VERTEX_POINT ( 'NONE', #18333 ) ;
#17078 = CARTESIAN_POINT ( 'NONE',  ( 47.05648932407426344, 97.58445800887258770, 31.27175355779120025 ) ) ;
#17079 = CARTESIAN_POINT ( 'NONE',  ( 47.43856463449117911, 154.7297705074273040, 35.64915139335015937 ) ) ;
#17080 = CARTESIAN_POINT ( 'NONE',  ( 43.01140435219951286, 59.62977050742730967, 29.55568802177586463 ) ) ;
#17082 = CARTESIAN_POINT ( 'NONE',  ( 14.85320491933239317, 121.4429315054255909, 16.22795414098078126 ) ) ;
#17081 = CARTESIAN_POINT ( 'NONE',  ( 40.27526882409969033, 111.5651871740939782, 37.97664729208901946 ) ) ;
#17083 = CARTESIAN_POINT ( 'NONE',  ( 46.10157429594899270, 73.76049967264873430, 38.46393386101376421 ) ) ;
#17085 = CARTESIAN_POINT ( 'NONE',  ( 44.55648932407425633, 135.6844580088725820, 38.96596240072933170 ) ) ;
#17084 = CARTESIAN_POINT ( 'NONE',  ( 38.01140435219952707, 10.71049967264875491, 34.21067981925357060 ) ) ;
#17086 = AXIS2_PLACEMENT_3D ( 'NONE', #14105, #12565, #5732 ) ;
#17087 = CARTESIAN_POINT ( 'NONE',  ( 41.46631938032478359, 124.3104996726487457, 38.96596240072933170 ) ) ;
#17088 = CARTESIAN_POINT ( 'NONE',  ( 43.34266540673962709, 94.90707761860556957, 39.21067981925357060 ) ) ;
#17089 = CARTESIAN_POINT ( 'NONE',  ( 43.01140435219951286, 74.36518717409400381, 29.55568802177586463 ) ) ;
#17090 = CARTESIAN_POINT ( 'NONE',  ( 42.68462674639443577, 144.9070776186055980, 29.21067981925357770 ) ) ;
#17091 = CARTESIAN_POINT ( 'NONE',  ( -151.4692556286852891, -181.1438272943107393, 59.56931450028537967 ) ) ;
#17092 = DIRECTION ( 'NONE',  ( 1.000000000000000000, 0.000000000000000000, 0.000000000000000000 ) ) ;
#17093 = VERTEX_POINT ( 'NONE', #3234 ) ;
#17094 = CARTESIAN_POINT ( 'NONE',  ( -148.5561028927606344, -189.0584106276440650, 40.69124936498395328 ) ) ;
#17095 = CARTESIAN_POINT ( 'NONE',  ( 26.66797635711824199, 149.9459070286683868, 17.30505193804556185 ) ) ;
#17096 = CARTESIAN_POINT ( 'NONE',  ( -159.0959885057557983, -175.8584106276440480, 55.19815736654470584 ) ) ;
#17097 = ORIENTED_EDGE ( 'NONE', *, *, #20616, .F. ) ;
#17098 = CARTESIAN_POINT ( 'NONE',  ( 47.43856463449117200, 139.7651871740939953, 32.77220824515698183 ) ) ;
#17099 = DIRECTION ( 'NONE',  ( 0.8660254037844388186, 0.000000000000000000, -0.4999999999999996114 ) ) ;
#17100 = CARTESIAN_POINT ( 'NONE',  ( 41.64333658814960870, 105.9797705074273182, 38.42115945441014446 ) ) ;
#17101 = CARTESIAN_POINT ( 'NONE',  ( 13.33420504782278293, 102.8437529505761603, 1.505736668420971869 ) ) ;
#17102 = VERTEX_POINT ( 'NONE', #9966 ) ;
#17103 = CARTESIAN_POINT ( 'NONE',  ( 27.10205971394288582, 96.62443569844734270, -5.915007788698968483 ) ) ;
#17104 = VECTOR ( 'NONE', #14557, 1000.000000000000000 ) ;
#17105 = VERTEX_POINT ( 'NONE', #8309 ) ;
#17106 = CARTESIAN_POINT ( 'NONE',  ( 43.01140435219951286, 100.4604996726487371, 39.21067981925356349 ) ) ;
#17107 = CARTESIAN_POINT ( 'NONE',  ( 43.01140435219957681, 96.53445800887259054, 39.21067981925356349 ) ) ;
#17108 = CARTESIAN_POINT ( 'NONE',  ( 47.43856463449117200, 83.02977050742730114, 32.77220824515698183 ) ) ;
#17109 = CARTESIAN_POINT ( 'NONE',  ( 44.37947211624943833, 148.0151871740940237, 38.42115945441014446 ) ) ;
#17110 =( BOUNDED_CURVE ( )  B_SPLINE_CURVE ( 2, ( #5731, #12343, #13997, #9052, #15650, #5013, #10595, #11721, #20732, #18344, #15031, #3247, #18754 ),
 .UNSPECIFIED., .F., .F. ) 
 B_SPLINE_CURVE_WITH_KNOTS ( ( 3, 2, 2, 2, 2, 2, 3 ),
 ( 0.4926470588235293824, 0.4941176470588235503, 0.4970588235294117752, 0.5000000000000000000, 0.5029411764705882248, 0.5058823529411764497, 0.5073529411764705621 ),
 .UNSPECIFIED. ) 
 CURVE ( )  GEOMETRIC_REPRESENTATION_ITEM ( )  RATIONAL_B_SPLINE_CURVE ( ( 0.9755282581475768211, 0.9755282581475763770, 1.000000000000000000, 0.9510565162951535312, 1.000000000000000000, 0.9510565162951535312, 1.000000000000000000, 0.9510565162951535312, 1.000000000000000000, 0.9510565162951535312, 1.000000000000000000, 0.9755282581475768211, 0.9755282581475768211 ) ) 
 REPRESENTATION_ITEM ( '' )  );
#17111 = CARTESIAN_POINT ( 'NONE',  ( 36.38086904327614235, 86.32171732562966326, 0.5532606071062302622 ) ) ;
#17112 = CARTESIAN_POINT ( 'NONE',  ( 46.10157429594899270, 118.7604996726487201, 38.46393386101375711 ) ) ;
#17113 = CARTESIAN_POINT ( 'NONE',  ( -148.3790856849358306, -166.5891397928654669, 59.16757674456786020 ) ) ;
#17114 = AXIS2_PLACEMENT_3D ( 'NONE', #14515, #12541, #4059 ) ;
#17115 = DIRECTION ( 'NONE',  ( -0.000000000000000000, -0.000000000000000000, 1.000000000000000000 ) ) ;
#17116 = FACE_BOUND ( 'NONE', #3776, .T. ) ;
#17117 = CARTESIAN_POINT ( 'NONE',  ( 116.4417310231185780, -126.9891397928655010, 0.3429884183836981459 ) ) ;
#17118 = AXIS2_PLACEMENT_3D ( 'NONE', #19485, #21150, #16061 ) ;
#17119 = CARTESIAN_POINT ( 'NONE',  ( 173.3794444120442506, -34.13255853780189142, 20.00000000000001776 ) ) ;
#17120 = EDGE_CURVE ( 'NONE', #21052, #17262, #17316, .T. ) ;
#17121 = CARTESIAN_POINT ( 'NONE',  ( 47.43856463449118621, 88.87977050742732388, 34.21067981925357060 ) ) ;
#17122 = CARTESIAN_POINT ( 'NONE',  ( 69.45715107853048664, 110.1171555912624740, -7.938611875467805667 ) ) ;
#17123 = CARTESIAN_POINT ( 'NONE',  ( -143.8425227516148084, -171.6938272943107222, 55.19815736654470584 ) ) ;
#17124 = CARTESIAN_POINT ( 'NONE',  ( 38.58424406990785371, 75.26518717409399528, 35.64915139335015937 ) ) ;
#17125 = CARTESIAN_POINT ( 'NONE',  ( 43.01140435219951996, 10.71049967264875491, 39.21067981925356349 ) ) ;
#17126 = CARTESIAN_POINT ( 'NONE',  ( -159.5594255724347761, -158.7891397928654555, 43.77915905869157598 ) ) ;
#17127 = VERTEX_POINT ( 'NONE', #19096 ) ;
#17128 = CARTESIAN_POINT ( 'NONE',  ( -145.2889157411863437, -189.5391397928653987, 41.15050349809589392 ) ) ;
#17129 = CYLINDRICAL_SURFACE ( 'NONE', #11318, 4.999999999999997335 ) ;
#17130 = CARTESIAN_POINT ( 'NONE',  ( 54.06307869441068448, 152.2224424482157303, -15.79932498977872868 ) ) ;
#17131 = EDGE_LOOP ( 'NONE', ( #15331, #1775, #8991, #9714 ) ) ;
#17132 = CARTESIAN_POINT ( 'NONE',  ( 47.43856463449117911, 62.02977050742732246, 32.77220824515697473 ) ) ;
#17133 = ORIENTED_EDGE ( 'NONE', *, *, #11208, .F. ) ;
#17134 = VECTOR ( 'NONE', #5832, 1000.000000000000000 ) ;
#17135 = CARTESIAN_POINT ( 'NONE',  ( 45.74753988029933538, 133.4297705074273210, 37.97664729208901946 ) ) ;
#17136 = DIRECTION ( 'NONE',  ( -0.000000000000000000, 1.000000000000000000, -0.000000000000000000 ) ) ;
#17137 = CARTESIAN_POINT ( 'NONE',  ( 38.58424406990784661, 62.96518717409399812, 32.77220824515698183 ) ) ;
#17138 = CARTESIAN_POINT ( 'NONE',  ( -142.0420953463936087, -195.5261189609773851, 49.65701158161630957 ) ) ;
#17139 = AXIS2_PLACEMENT_3D ( 'NONE', #3590, #10318, #17020 ) ;
#17140 = CARTESIAN_POINT ( 'NONE',  ( 38.58424406990784661, 96.26518717409400949, 35.64915139335016647 ) ) ;
#17141 = CARTESIAN_POINT ( 'NONE',  ( -141.4692556286852891, -173.9130981290893203, 46.40781461928724383 ) ) ;
#17142 = LINE ( 'NONE', #6814, #6884 ) ;
#17143 = CARTESIAN_POINT ( 'NONE',  ( -159.5594255724347761, -166.8630981290893089, 43.77915905869157598 ) ) ;
#17144 = DIRECTION ( 'NONE',  ( 0.000000000000000000, 0.000000000000000000, 1.000000000000000000 ) ) ;
#17145 = CARTESIAN_POINT ( 'NONE',  ( 43.80332655382221674, 109.9575765865523067, 29.21067981925357060 ) ) ;
#17146 = CARTESIAN_POINT ( 'NONE',  ( 38.96631938032478359, 140.4844580088725650, 31.27175355779120025 ) ) ;
#17147 = CARTESIAN_POINT ( 'NONE',  ( 44.37947211624943833, 122.4797705074273182, 30.00020018409699318 ) ) ;
#17148 = CARTESIAN_POINT ( 'NONE',  ( 26.43292637418678126, 142.8198486544370098, 2.223537717183381002 ) ) ;
#17149 = DIRECTION ( 'NONE',  ( 1.000000000000000000, 0.000000000000000000, 0.000000000000000000 ) ) ;
#17150 = CARTESIAN_POINT ( 'NONE',  ( 44.37947211624943833, 106.0151871740939953, 38.42115945441014446 ) ) ;
#17151 = CARTESIAN_POINT ( 'NONE',  ( 39.92123440845005433, 126.2344580088725934, 38.46393386101375711 ) ) ;
#17152 = CARTESIAN_POINT ( 'NONE',  ( 77.22348061889915982, 118.7203125366680752, -8.375138532479306619 ) ) ;
#17153 = CARTESIAN_POINT ( 'NONE',  ( 25.21830160582964453, 141.7844325674071229, 10.15653385063274428 ) ) ;
#17154 = DIRECTION ( 'NONE',  ( -0.000000000000000000, -0.000000000000000000, -1.000000000000000000 ) ) ;
#17155 = ADVANCED_FACE ( 'NONE', ( #7197 ), #20745, .T. ) ;
#17156 = CARTESIAN_POINT ( 'NONE',  ( 40.27526882409969744, 83.92977050742732104, 30.44471234641812174 ) ) ;
#17157 = EDGE_CURVE ( 'NONE', #17262, #13406, #15246, .T. ) ;
#17158 = AXIS2_PLACEMENT_3D ( 'NONE', #14928, #8009, #11080 ) ;
#17159 = CARTESIAN_POINT ( 'NONE',  ( 41.46631938032478359, 77.18445800887258201, 29.45539723777780239 ) ) ;
#17160 = CARTESIAN_POINT ( 'NONE',  ( -136.4581486297550441, -116.9891397928655010, 49.65701158161631668 ) ) ;
#17161 = VECTOR ( 'NONE', #16847, 1000.000000000000114 ) ;
#17162 = CARTESIAN_POINT ( 'NONE',  ( 38.01140435219952707, 129.7104996726487514, 34.21067981925357060 ) ) ;
#17164 = CARTESIAN_POINT ( 'NONE',  ( 66.98923854426821833, 144.2286169274386509, -8.299483363615854259 ) ) ;
#17163 = CARTESIAN_POINT ( 'NONE',  ( 43.01140435219951286, 84.86518717409398960, 38.86567161673127657 ) ) ;
#17165 = CARTESIAN_POINT ( 'NONE',  ( -143.8425227516148084, -162.3584106276440480, 44.11586579668791330 ) ) ;
#17166 = CARTESIAN_POINT ( 'NONE',  ( -148.5561028927606344, -185.7938272943107449, 40.69124936498395328 ) ) ;
#17167 = DIRECTION ( 'NONE',  ( 0.000000000000000000, 0.000000000000000000, 1.000000000000000000 ) ) ;
#17168 = CARTESIAN_POINT ( 'NONE',  ( -154.5594255724347761, -192.9630981290893317, 59.16757674456785310 ) ) ;
#17169 = DIRECTION ( 'NONE',  ( 1.000000000000000000, 0.000000000000000000, 0.000000000000000000 ) ) ;
#17170 = FACE_BOUND ( 'NONE', #8830, .T. ) ;
#17171 = CARTESIAN_POINT ( 'NONE',  ( 43.01140435219954838, 110.0344580088725763, 29.21067981925356705 ) ) ;
#17172 = CARTESIAN_POINT ( 'NONE',  ( 47.43856463449117200, 148.7297705074273324, 35.64915139335016647 ) ) ;
#17173 = CARTESIAN_POINT ( 'NONE',  ( 44.37947211624943833, 101.4797705074273182, 30.00020018409699318 ) ) ;
#17174 = CARTESIAN_POINT ( 'NONE',  ( 38.54497605562327323, 85.96704844161884296, 14.48200433579215662 ) ) ;
#17175 = CARTESIAN_POINT ( 'NONE',  ( 46.59305225739526435, 136.9151871740940010, 31.60846029578754468 ) ) ;
#17176 = DIRECTION ( 'NONE',  ( 0.000000000000000000, -1.000000000000000000, 0.000000000000000000 ) ) ;
#17177 = CARTESIAN_POINT ( 'NONE',  ( -154.3824083646099439, -166.5584106276440366, 58.62277379824867296 ) ) ;
#17178 = DIRECTION ( 'NONE',  ( 0.000000000000000000, 0.000000000000000000, 1.000000000000000000 ) ) ;
#17179 = CARTESIAN_POINT ( 'NONE',  ( 14.87688376430095616, 117.0300574687981481, 8.056989239287382532 ) ) ;
#17180 = CARTESIAN_POINT ( 'NONE',  ( 43.01140435219951996, 10.71049967264875491, 39.21067981925356349 ) ) ;
#17181 = CARTESIAN_POINT ( 'NONE',  ( 38.58424406990786082, 114.1151871740939896, 34.21067981925357060 ) ) ;
#17182 = ORIENTED_EDGE ( 'NONE', *, *, #17559, .T. ) ;
#17183 = CARTESIAN_POINT ( 'NONE',  ( -120.0322075325610598, -126.9891397928655010, -34.99999999999999289 ) ) ;
#17184 = EDGE_LOOP ( 'NONE', ( #4795, #16501, #8951, #3013 ) ) ;
#17185 = CARTESIAN_POINT ( 'NONE',  ( 38.01140435219952707, 101.7844580088725905, 34.21067981925357060 ) ) ;
#17186 = CARTESIAN_POINT ( 'NONE',  ( 45.74753988029934249, 152.3297705074272983, 30.44471234641812174 ) ) ;
#17187 = CARTESIAN_POINT ( 'NONE',  ( 47.43856463449117200, 61.72977050742730398, 35.64915139335016647 ) ) ;
#17189 = CARTESIAN_POINT ( 'NONE',  ( 34.40470276422951912, 146.6778736915268553, -16.43444041970612446 ) ) ;
#17188 = CARTESIAN_POINT ( 'NONE',  ( 41.64333658814960870, 111.7151871740940123, 38.42115945441014446 ) ) ;
#17190 = CARTESIAN_POINT ( 'NONE',  ( 38.01140435219951996, 69.56049967264873146, 32.58608133808903773 ) ) ;
#17192 = CARTESIAN_POINT ( 'NONE',  ( 46.10157429594899270, 148.7344580088725934, 29.95742577749336988 ) ) ;
#17191 = CARTESIAN_POINT ( 'NONE',  ( 45.07664058499605630, 144.8220846865936551, 29.65421901078121536 ) ) ;
#17193 = B_SPLINE_CURVE_WITH_KNOTS ( 'NONE', 3,
 ( #8972, #15786, #20653, #12264, #5755, #12484, #5651, #10521 ),
 .UNSPECIFIED., .F., .F.,
 ( 4, 2, 2, 4 ),
 ( 0.002864483144845920114, 0.004294853615569176747, 0.005010038850930815038, 0.005725224086292454197 ),
 .UNSPECIFIED. ) ;
#17194 = CARTESIAN_POINT ( 'NONE',  ( -40.97538603781489996, -6.141859983696321912, -35.00000000000000000 ) ) ;
#17195 = CYLINDRICAL_SURFACE ( 'NONE', #1295, 4.999999999999997335 ) ;
#17196 = CARTESIAN_POINT ( 'NONE',  ( 39.42975644700377558, 81.41518717409400097, 36.81289934271958941 ) ) ;
#17197 = CARTESIAN_POINT ( 'NONE',  ( 48.01140435219951996, 104.0604996726487457, 35.83527830041809636 ) ) ;
#17198 = CARTESIAN_POINT ( 'NONE',  ( -157.2955611005346270, -178.4438272943107222, 57.67623309621198047 ) ) ;
#17199 = ORIENTED_EDGE ( 'NONE', *, *, #4945, .T. ) ;
#17200 = CARTESIAN_POINT ( 'NONE',  ( 59.73150498404358899, 90.03452709159309109, 13.76780503130795097 ) ) ;
#17201 = ORIENTED_EDGE ( 'NONE', *, *, #9756, .T. ) ;
#17202 = CARTESIAN_POINT ( 'NONE',  ( 38.58424406990786082, 147.1151871740939896, 34.21067981925357060 ) ) ;
#17203 = DIRECTION ( 'NONE',  ( -0.000000000000000000, -0.000000000000000000, 1.000000000000000000 ) ) ;
#17204 = CARTESIAN_POINT ( 'NONE',  ( 41.64333658814960870, 108.9797705074273324, 38.42115945441014446 ) ) ;
#17205 = CARTESIAN_POINT ( 'NONE',  ( 77.22939692449374149, 120.9137088693742044, 5.553548964694690504 ) ) ;
#17206 = ORIENTED_EDGE ( 'NONE', *, *, #20919, .T. ) ;
#17207 = VECTOR ( 'NONE', #14725, 1000.000000000000000 ) ;
#17208 = CARTESIAN_POINT ( 'NONE',  ( 19.85370653151704090, 103.8158566922722486, 8.489678972899794118 ) ) ;
#17209 = EDGE_LOOP ( 'NONE', ( #10264, #1361, #18425, #2254, #3594, #12473 ) ) ;
#17210 = CARTESIAN_POINT ( 'NONE',  ( -151.4692556286852607, -191.3130981290892976, 39.65701158161629536 ) ) ;
#17211 = CARTESIAN_POINT ( 'NONE',  ( 44.55648932407425633, 88.61049967264874283, 38.96596240072933170 ) ) ;
#17212 = CARTESIAN_POINT ( 'NONE',  ( 38.58424406990786082, 84.37977050742730967, 34.21067981925357060 ) ) ;
#17213 = CARTESIAN_POINT ( 'NONE',  ( 47.43856463449118621, 142.6151871740939896, 34.21067981925357060 ) ) ;
#17214 = CARTESIAN_POINT ( 'NONE',  ( 41.46631938032478359, 99.11049967264872862, 29.45539723777780239 ) ) ;
#17215 = CARTESIAN_POINT ( 'NONE',  ( 32.98198692859195802, 152.6383102900375093, -3.493975233523312962 ) ) ;
#17216 = CARTESIAN_POINT ( 'NONE',  ( 43.01140435219951286, 61.46049967264873715, 39.21067981925356349 ) ) ;
#17217 = CARTESIAN_POINT ( 'NONE',  ( -145.2889157411863721, -169.4391397928654044, 58.16351966513671812 ) ) ;
#17218 = CARTESIAN_POINT ( 'NONE',  ( -151.4692556286852891, -188.3130981290893260, 39.65701158161630246 ) ) ;
#17219 = UNCERTAINTY_MEASURE_WITH_UNIT (LENGTH_MEASURE( 1.000000000000000082E-05 ), #19634, 'distance_accuracy_value', 'NONE');
#17220 = CARTESIAN_POINT ( 'NONE',  ( 10.61900875472251649, 108.8314319666055212, -5.279948415675857376 ) ) ;
#17221 = CARTESIAN_POINT ( 'NONE',  ( 43.01140435219951286, 65.03445800887257633, 29.21067981925356705 ) ) ;
#17222 = LINE ( 'NONE', #11729, #2187 ) ;
#17223 = CIRCLE ( 'NONE', #18291, 16.96660865288809816 ) ;
#17224 = CARTESIAN_POINT ( 'NONE',  ( 47.43856463449117200, 89.02977050742731535, 32.77220824515698183 ) ) ;
#17225 = CARTESIAN_POINT ( 'NONE',  ( -159.0959885057557983, -178.5938272943107279, 55.19815736654470584 ) ) ;
#17226 = CARTESIAN_POINT ( 'NONE',  ( 38.58424406990786082, 78.11518717409400381, 34.21067981925357060 ) ) ;
#17227 = LINE ( 'NONE', #13606, #15892 ) ;
#17228 = DIRECTION ( 'NONE',  ( -0.000000000000000000, -0.000000000000000000, -1.000000000000000000 ) ) ;
#17229 = ORIENTED_EDGE ( 'NONE', *, *, #15831, .F. ) ;
#17230 = CARTESIAN_POINT ( 'NONE',  ( 41.46631938032478359, 69.38445800887258486, 38.96596240072933170 ) ) ;
#17231 = DIRECTION ( 'NONE',  ( 0.000000000000000000, 1.000000000000000000, 0.000000000000000000 ) ) ;
#17232 = CARTESIAN_POINT ( 'NONE',  ( 47.43856463449117911, 133.7297705074273324, 35.64915139335015937 ) ) ;
#17233 = CARTESIAN_POINT ( 'NONE',  ( 63.68221904981356829, 147.0951523173380338, -15.44234037292825690 ) ) ;
#17234 = ORIENTED_EDGE ( 'NONE', *, *, #16906, .T. ) ;
#17235 = FILL_AREA_STYLE ('',( #2151 ) ) ;
#17236 =( BOUNDED_CURVE ( )  B_SPLINE_CURVE ( 2, ( #388, #10956, #7117, #17343, #2250, #20562, #8985, #15691, #597, #17448, #2357, #9096, #15797 ),
 .UNSPECIFIED., .F., .F. ) 
 B_SPLINE_CURVE_WITH_KNOTS ( ( 3, 2, 2, 2, 2, 2, 3 ),
 ( 0.4044117647058823595, 0.4058823529411764719, 0.4088235294117646967, 0.4117647058823529216, 0.4147058823529412019, 0.4176470588235294268, 0.4191176470588235392 ),
 .UNSPECIFIED. ) 
 CURVE ( )  GEOMETRIC_REPRESENTATION_ITEM ( )  RATIONAL_B_SPLINE_CURVE ( ( 0.9755282581475768211, 0.9755282581475768211, 1.000000000000000000, 0.9510565162951535312, 1.000000000000000000, 0.9510565162951535312, 1.000000000000000000, 0.9510565162951535312, 1.000000000000000000, 0.9510565162951535312, 1.000000000000000000, 0.9755282581475768211, 0.9755282581475768211 ) ) 
 REPRESENTATION_ITEM ( '' )  );
#17237 = ORIENTED_EDGE ( 'NONE', *, *, #6350, .F. ) ;
#17238 = CARTESIAN_POINT ( 'NONE',  ( 41.64333658814960870, 131.7797705074273154, 30.00020018409699318 ) ) ;
#17239 =( GEOMETRIC_REPRESENTATION_CONTEXT ( 3 ) GLOBAL_UNCERTAINTY_ASSIGNED_CONTEXT ( ( #15261 ) ) GLOBAL_UNIT_ASSIGNED_CONTEXT ( ( #12975, #11309, #19477 ) ) REPRESENTATION_CONTEXT ( 'NONE', 'WORKASPACE' ) );
#17240 = CARTESIAN_POINT ( 'NONE',  ( 43.01140435219951286, 92.62977050742732388, 29.55568802177586463 ) ) ;
#17241 = CARTESIAN_POINT ( 'NONE',  ( -141.4692556286852891, -180.9891397928654726, 49.65701158161630957 ) ) ;
#17242 = LINE ( 'NONE', #20250, #10104 ) ;
#17243 = CARTESIAN_POINT ( 'NONE',  ( 111.4021762516569964, 137.5714195593754710, -19.99999999999997868 ) ) ;
#17244 = CARTESIAN_POINT ( 'NONE',  ( -151.4692556286852607, -191.3130981290892976, 39.65701158161629536 ) ) ;
#17245 = CARTESIAN_POINT ( 'NONE',  ( 46.59305225739526435, 100.3151871740940067, 36.81289934271958941 ) ) ;
#17246 = CARTESIAN_POINT ( 'NONE',  ( 39.92123440845005433, 153.2604996726487343, 29.95742577749336988 ) ) ;
#17247 = CARTESIAN_POINT ( 'NONE',  ( -151.4692556286852607, -171.8130981290892976, 59.65701158161632378 ) ) ;
#17248 = CARTESIAN_POINT ( 'NONE',  ( -141.4692556286852891, -171.0630981290893260, 49.65701158161630957 ) ) ;
#17249 = LINE ( 'NONE', #507, #10039 ) ;
#17250 = CARTESIAN_POINT ( 'NONE',  ( 48.01140435219951996, 142.2844580088725763, 34.21067981925357060 ) ) ;
#17251 = CARTESIAN_POINT ( 'NONE',  ( 41.64333658814960870, 113.7797705074273296, 30.00020018409699318 ) ) ;
#17252 = CARTESIAN_POINT ( 'NONE',  ( 42.43310160994198554, 85.59785666124599857, 20.35848333119881914 ) ) ;
#17253 = CARTESIAN_POINT ( 'NONE',  ( 38.96631938032478359, 141.0844580088725877, 37.14960608071593384 ) ) ;
#17254 = CARTESIAN_POINT ( 'NONE',  ( 40.27526882409969744, 107.6651871740940152, 30.44471234641812174 ) ) ;
#17255 = ORIENTED_EDGE ( 'NONE', *, *, #20635, .F. ) ;
#17256 = AXIS2_PLACEMENT_3D ( 'NONE', #20852, #5742, #7522 ) ;
#17257 = CARTESIAN_POINT ( 'NONE',  ( 138.2149183826930425, 102.3264679885537305, 14.00000000000001776 ) ) ;
#17258 = CARTESIAN_POINT ( 'NONE',  ( 12.60192345832597027, 135.3850619972812979, 10.60811072801600119 ) ) ;
#17259 = CARTESIAN_POINT ( 'NONE',  ( 69.49396330798431620, 129.5978393632817927, 5.275421687385184910 ) ) ;
#17260 = CARTESIAN_POINT ( 'NONE',  ( 43.01140435219951996, 10.71049967264875491, 39.21067981925356349 ) ) ;
#17261 = CARTESIAN_POINT ( 'NONE',  ( 46.59305225739526435, 85.57977050742732672, 36.81289934271958941 ) ) ;
#17262 = VERTEX_POINT ( 'NONE', #3778 ) ;
#17263 = PRODUCT_DEFINITION ( 'UNKNOWN', '', #20424, #16982 ) ;
#17264 = CARTESIAN_POINT ( 'NONE',  ( 46.10157429594899270, 67.73445800887256496, 29.95742577749337343 ) ) ;
#17265 = DIRECTION ( 'NONE',  ( -0.5000000000000004441, 0.000000000000000000, -0.8660254037844383745 ) ) ;
#17267 = EDGE_CURVE ( 'NONE', #19734, #1249, #9923, .T. ) ;
#17266 = CARTESIAN_POINT ( 'NONE',  ( 39.92123440845004723, 130.1604996726487400, 38.46393386101376421 ) ) ;
#17269 = CARTESIAN_POINT ( 'NONE',  ( 9.647618190908266556, 112.6042302384299916, -11.15662622088235167 ) ) ;
#17268 = CARTESIAN_POINT ( 'NONE',  ( 41.64333658814960870, 90.71518717409401233, 38.42115945441014446 ) ) ;
#17270 = CARTESIAN_POINT ( 'NONE',  ( -151.4692556286852891, -160.4084106276440593, 59.56931450028537967 ) ) ;
#17271 = CARTESIAN_POINT ( 'NONE',  ( -143.8425227516148084, -177.6938272943107506, 55.19815736654470584 ) ) ;
#17272 = CARTESIAN_POINT ( 'NONE',  ( 41.46631938032478359, 117.3844580088725849, 38.96596240072933170 ) ) ;
#17273 = LINE ( 'NONE', #11780, #17739 ) ;
#17274 = CARTESIAN_POINT ( 'NONE',  ( 43.80332655382222384, 68.88361825032845331, 29.21067981925357770 ) ) ;
#17275 = DIRECTION ( 'NONE',  ( -0.000000000000000000, -0.000000000000000000, -1.000000000000000000 ) ) ;
#17276 = CARTESIAN_POINT ( 'NONE',  ( 38.58424406990784661, 141.5297705074272869, 35.64915139335016647 ) ) ;
#17277 = CARTESIAN_POINT ( 'NONE',  ( 47.43856463449117200, 100.7297705074273040, 35.64915139335016647 ) ) ;
#17278 = ADVANCED_FACE ( 'NONE', ( #8855 ), #8957, .T. ) ;
#17279 = CARTESIAN_POINT ( 'NONE',  ( 76.40658810299491677, 127.4365358892444959, 12.33923360994393903 ) ) ;
#17280 = CARTESIAN_POINT ( 'NONE',  ( 47.43856463449118621, 133.6151871740940180, 34.21067981925357060 ) ) ;
#17281 = DIRECTION ( 'NONE',  ( 1.000000000000000000, 0.000000000000000000, -1.186952418100008983E-16 ) ) ;
#17282 = CARTESIAN_POINT ( 'NONE',  ( -159.0959885057557983, -166.8584106276440480, 55.19815736654470584 ) ) ;
#17283 = CARTESIAN_POINT ( 'NONE',  ( 43.01140435219951286, 68.62977050742729546, 29.55568802177586463 ) ) ;
#17284 = CARTESIAN_POINT ( 'NONE',  ( 96.62434152388763664, 220.7958015105191976, -5.999999999999976019 ) ) ;
#17285 = CARTESIAN_POINT ( 'NONE',  ( 15.40311202476076780, 126.0397005259128065, 8.413886508562818278 ) ) ;
#17286 = ADVANCED_FACE ( 'NONE', ( #5522 ), #18983, .F. ) ;
#17287 = FACE_BOUND ( 'NONE', #9278, .T. ) ;
#17288 = CARTESIAN_POINT ( 'NONE',  ( 47.43856463449117200, 115.7651871740939811, 32.77220824515698183 ) ) ;
#17289 = ORIENTED_EDGE ( 'NONE', *, *, #17669, .T. ) ;
#17290 = FACE_OUTER_BOUND ( 'NONE', #2563, .T. ) ;
#17291 = VERTEX_POINT ( 'NONE', #12137 ) ;
#17292 = CARTESIAN_POINT ( 'NONE',  ( 41.46631938032478359, 104.1844580088725820, 29.45539723777780239 ) ) ;
#17293 = CIRCLE ( 'NONE', #8532, 7.500000000000007105 ) ;
#17294 =( REPRESENTATION_RELATIONSHIP ('NONE','NONE', #6933, #5457 ) REPRESENTATION_RELATIONSHIP_WITH_TRANSFORMATION ( #1265 )SHAPE_REPRESENTATION_RELATIONSHIP( ) );
#17295 = AXIS2_PLACEMENT_3D ( 'NONE', #7091, #10185, #249 ) ;
#17296 = CARTESIAN_POINT ( 'NONE',  ( 44.55648932407425633, 154.6104996726487570, 38.96596240072933170 ) ) ;
#17298 = CARTESIAN_POINT ( 'NONE',  ( 48.35156950851215640, 92.21792820573091376, 14.20396468032920012 ) ) ;
#17297 = CARTESIAN_POINT ( 'NONE',  ( 44.37947211624943833, 118.0151871740940095, 38.42115945441014446 ) ) ;
#17299 = CARTESIAN_POINT ( 'NONE',  ( 48.01140435219951996, 74.36049967264871441, 32.58608133808903773 ) ) ;
#17301 = CARTESIAN_POINT ( 'NONE',  ( 39.92123440845005433, 75.23445800887257917, 38.46393386101375711 ) ) ;
#17300 = CARTESIAN_POINT ( 'NONE',  ( 46.98624069623303967, 144.5897511595969149, 31.15999777443385810 ) ) ;
#17302 = EDGE_CURVE ( 'NONE', #2927, #6406, #3565, .T. ) ;
#17303 = CARTESIAN_POINT ( 'NONE',  ( -153.0531000319306827, -171.8899795514095672, 59.65701158161631668 ) ) ;
#17304 = DIRECTION ( 'NONE',  ( -1.000000000000000000, 0.000000000000000000, 0.000000000000000000 ) ) ;
#17305 = CARTESIAN_POINT ( 'NONE',  ( 39.42975644700377558, 80.81518717409400665, 31.60846029578754468 ) ) ;
#17306 = CARTESIAN_POINT ( 'NONE',  ( 44.55648932407425633, 103.6104996726487428, 38.96596240072933170 ) ) ;
#17307 = CARTESIAN_POINT ( 'NONE',  ( -154.3824083646099439, -176.4938272943107336, 40.69124936498395328 ) ) ;
#17308 = CARTESIAN_POINT ( 'NONE',  ( -159.0959885057557983, -193.8584106276440480, 55.19815736654470584 ) ) ;
#17309 = ORIENTED_EDGE ( 'NONE', *, *, #21498, .F. ) ;
#17310 = CARTESIAN_POINT ( 'NONE',  ( -142.0420953463935803, -177.8084106276440650, 52.72008163687743831 ) ) ;
#17311 = CARTESIAN_POINT ( 'NONE',  ( 66.79148812173782801, 144.6461433805978061, 3.691718863876278345 ) ) ;
#17312 = ORIENTED_EDGE ( 'NONE', *, *, #6100, .F. ) ;
#17313 = CIRCLE ( 'NONE', #9589, 3.000000000000000444 ) ;
#17314 = CARTESIAN_POINT ( 'NONE',  ( 46.59305225739526435, 145.9151871740940294, 31.60846029578754468 ) ) ;
#17315 = AXIS2_PLACEMENT_3D ( 'NONE', #20506, #15748, #15848 ) ;
#17316 = LINE ( 'NONE', #10507, #19411 ) ;
#17317 = CARTESIAN_POINT ( 'NONE',  ( 40.27526882409969744, 102.8297705074273125, 37.97664729208901235 ) ) ;
#17318 = CARTESIAN_POINT ( 'NONE',  ( 50.92548328124963319, 86.60151408976496157, 0.07716523989554470442 ) ) ;
#17319 = VERTEX_POINT ( 'NONE', #10399 ) ;
#17320 = AXIS2_PLACEMENT_3D ( 'NONE', #16135, #4446, #14478 ) ;
#17321 = CARTESIAN_POINT ( 'NONE',  ( 66.49460585200260709, 135.5194395740885511, -1.986604139701473759 ) ) ;
#17322 = EDGE_LOOP ( 'NONE', ( #15829, #5772, #5557 ) ) ;
#17323 = CARTESIAN_POINT ( 'NONE',  ( 40.27526882409969033, 110.9297705074272926, 30.44471234641811819 ) ) ;
#17324 = CYLINDRICAL_SURFACE ( 'NONE', #21444, 10.00000000000000888 ) ;
#17325 = CARTESIAN_POINT ( 'NONE',  ( 43.01140435219951996, 147.5344580088726048, 39.21067981925356349 ) ) ;
#17326 = EDGE_CURVE ( 'NONE', #12850, #20510, #10964, .T. ) ;
#17327 = CARTESIAN_POINT ( 'NONE',  ( 47.43856463449117200, 82.72977050742731819, 35.64915139335016647 ) ) ;
#17328 = CARTESIAN_POINT ( 'NONE',  ( 47.43856463449117200, 145.4651871740939839, 35.64915139335016647 ) ) ;
#17329 = CARTESIAN_POINT ( 'NONE',  ( 38.01140435219951996, 96.86049967264871441, 35.83527830041810347 ) ) ;
#17330 = CARTESIAN_POINT ( 'NONE',  ( 23.67598417054553295, 91.65793073385727041, -5.994147020910363999 ) ) ;
#17331 = CARTESIAN_POINT ( 'NONE',  ( 48.01140435219951996, 119.0604996726487315, 35.83527830041809636 ) ) ;
#17332 = CARTESIAN_POINT ( 'NONE',  ( -151.4692556286852891, -166.7391397928654442, 60.17163382399899518 ) ) ;
#17333 = CARTESIAN_POINT ( 'NONE',  ( 156.5548063637509415, 177.1359029563629406, -44.99999999999997158 ) ) ;
#17334 = DIRECTION ( 'NONE',  ( 1.000000000000000000, 0.000000000000000000, 0.000000000000000000 ) ) ;
#17335 = DIRECTION ( 'NONE',  ( 0.000000000000000000, 1.000000000000000000, 0.000000000000000000 ) ) ;
#17336 = ORIENTED_EDGE ( 'NONE', *, *, #3727, .F. ) ;
#17337 = CARTESIAN_POINT ( 'NONE',  ( 45.74753988029933538, 80.32977050742731251, 30.44471234641811819 ) ) ;
#17338 = CARTESIAN_POINT ( 'NONE',  ( -157.2955611005346270, -160.4438272943106654, 57.67623309621198047 ) ) ;
#17339 = CARTESIAN_POINT ( 'NONE',  ( 41.64333658814960870, 77.51518717409399528, 30.00020018409699318 ) ) ;
#17340 = CARTESIAN_POINT ( 'NONE',  ( 77.22348061889915982, 118.7203125366680752, -8.375138532479306619 ) ) ;
#17341 = CARTESIAN_POINT ( 'NONE',  ( -148.5561028927606344, -195.0584106276440650, 40.69124936498395328 ) ) ;
#17342 = ORIENTED_EDGE ( 'NONE', *, *, #11249, .T. ) ;
#17343 = CARTESIAN_POINT ( 'NONE',  ( 39.92123440845005433, 118.1604996726487400, 38.46393386101375711 ) ) ;
#17344 = CARTESIAN_POINT ( 'NONE',  ( 39.42975644700377558, 129.0797705074273267, 31.60846029578754468 ) ) ;
#17345 = CARTESIAN_POINT ( 'NONE',  ( 39.14927582833848874, 92.05416703502255871, 8.565614722876343734 ) ) ;
#17346 = ORIENTED_EDGE ( 'NONE', *, *, #9259, .T. ) ;
#17347 = CARTESIAN_POINT ( 'NONE',  ( -151.4692556286852891, -196.9891397928655010, 59.65701158161632378 ) ) ;
#17348 = ORIENTED_EDGE ( 'NONE', *, *, #21147, .T. ) ;
#17349 = CARTESIAN_POINT ( 'NONE',  ( 47.43856463449117200, 134.0297705074273154, 32.77220824515698183 ) ) ;
#17350 = EDGE_CURVE ( 'NONE', #15251, #16317, #16993, .T. ) ;
#17351 = CARTESIAN_POINT ( 'NONE',  ( 47.43856463449117200, 91.72977050742730398, 35.64915139335016647 ) ) ;
#17352 = DIRECTION ( 'NONE',  ( 1.000000000000000000, 0.000000000000000000, 0.000000000000000000 ) ) ;
#17353 = FACE_OUTER_BOUND ( 'NONE', #792, .T. ) ;
#17354 = CARTESIAN_POINT ( 'NONE',  ( 163.2398440670430944, 192.0365442723309570, 23.61216616543570979 ) ) ;
#17355 = EDGE_CURVE ( 'NONE', #10804, #11596, #21184, .T. ) ;
#17356 = CARTESIAN_POINT ( 'NONE',  ( 41.64333658814960870, 101.5151871740939953, 30.00020018409699318 ) ) ;
#17357 = CARTESIAN_POINT ( 'NONE',  ( -149.8854112254399240, -174.7362167067690280, 59.65701158161632378 ) ) ;
#17358 = CARTESIAN_POINT ( 'NONE',  ( -151.4692556286852891, -196.9891397928655010, 49.65701158161630957 ) ) ;
#17359 = CARTESIAN_POINT ( 'NONE',  ( -145.2889157411863721, -159.5130981290892578, 58.16351966513671812 ) ) ;
#17360 = DIRECTION ( 'NONE',  ( 0.000000000000000000, 0.000000000000000000, 1.000000000000000000 ) ) ;
#17361 = CARTESIAN_POINT ( 'NONE',  ( 47.05648932407426344, 132.9844580088725934, 37.14960608071593384 ) ) ;
#17362 = CARTESIAN_POINT ( 'NONE',  ( 46.59305225739526435, 115.5797705074273267, 36.81289934271958941 ) ) ;
#17363 = CARTESIAN_POINT ( 'NONE',  ( 66.29928749942908439, 103.8601778506706239, 12.34270352495849110 ) ) ;
#17364 = CARTESIAN_POINT ( 'NONE',  ( -142.0420953463935803, -192.5438272943107449, 52.72008163687743831 ) ) ;
#17365 = CARTESIAN_POINT ( 'NONE',  ( 40.27526882409969744, 111.5651871740939782, 37.97664729208901235 ) ) ;
#17366 = ORIENTED_EDGE ( 'NONE', *, *, #3797, .T. ) ;
#17367 = DIRECTION ( 'NONE',  ( -0.000000000000000000, -0.000000000000000000, -1.000000000000000000 ) ) ;
#17368 = CARTESIAN_POINT ( 'NONE',  ( 32.98198692859195802, 152.6383102900375093, -3.493975233523312962 ) ) ;
#17369 =( BOUNDED_CURVE ( )  B_SPLINE_CURVE ( 2, ( #4394, #12781, #19502, #7620, #20841, #19612, #15971, #14537, #21278, #12891, #5834, #16081, #4506 ),
 .UNSPECIFIED., .F., .F. ) 
 B_SPLINE_CURVE_WITH_KNOTS ( ( 3, 2, 2, 2, 2, 2, 3 ),
 ( 0.3897058823529411797, 0.3911764705882352922, 0.3941176470588235170, 0.3970588235294117418, 0.4000000000000000222, 0.4029411764705882470, 0.4044117647058823595 ),
 .UNSPECIFIED. ) 
 CURVE ( )  GEOMETRIC_REPRESENTATION_ITEM ( )  RATIONAL_B_SPLINE_CURVE ( ( 0.9755282581475768211, 0.9755282581475768211, 1.000000000000000000, 0.9510565162951535312, 1.000000000000000000, 0.9510565162951535312, 1.000000000000000000, 0.9510565162951535312, 1.000000000000000000, 0.9510565162951535312, 1.000000000000000000, 0.9755282581475768211, 0.9755282581475768211 ) ) 
 REPRESENTATION_ITEM ( '' )  );
#17370 = CARTESIAN_POINT ( 'NONE',  ( 30.72731853479779929, 94.52359049060457608, 14.91853181686295038 ) ) ;
#17371 = DIRECTION ( 'NONE',  ( 1.000000000000000000, 0.000000000000000000, -0.000000000000000000 ) ) ;
#17372 = CARTESIAN_POINT ( 'NONE',  ( 41.64333658814960870, 72.97977050742731819, 38.42115945441014446 ) ) ;
#17373 = VERTEX_POINT ( 'NONE', #18871 ) ;
#17374 = CARTESIAN_POINT ( 'NONE',  ( 38.96631938032478359, 65.48445800887257917, 31.27175355779120025 ) ) ;
#17375 = CARTESIAN_POINT ( 'NONE',  ( -141.4692556286852891, -171.9891397928654726, 49.65701158161630957 ) ) ;
#17376 = CARTESIAN_POINT ( 'NONE',  ( 47.05648932407426344, 127.9104996726487542, 37.14960608071593384 ) ) ;
#17378 = CARTESIAN_POINT ( 'NONE',  ( 39.81857293680397447, 85.90283706545402254, -5.561266875997713299 ) ) ;
#17377 = CARTESIAN_POINT ( 'NONE',  ( 38.58424406990784661, 80.96518717409399812, 32.77220824515698183 ) ) ;
#17379 = ADVANCED_FACE ( 'NONE', ( #8636 ), #15562, .F. ) ;
#17380 = CARTESIAN_POINT ( 'NONE',  ( -151.4692556286852891, -179.6438272943107108, 39.74470866294723947 ) ) ;
#17381 = CARTESIAN_POINT ( 'NONE',  ( 43.80332655382220253, 113.8836182503284533, 29.21067981925356705 ) ) ;
#17382 = CARTESIAN_POINT ( 'NONE',  ( -141.4692556286852891, -192.2130981290892748, 52.90620854394536821 ) ) ;
#17383 = CYLINDRICAL_SURFACE ( 'NONE', #8460, 4.999999999999997335 ) ;
#17384 = CARTESIAN_POINT ( 'NONE',  ( 38.96631938032478359, 93.08445800887257349, 37.14960608071593384 ) ) ;
#17385 = CARTESIAN_POINT ( 'NONE',  ( 47.05648932407426344, 143.5104996726487627, 31.27175355779120025 ) ) ;
#17386 = CARTESIAN_POINT ( 'NONE',  ( 38.58424406990784661, 144.5297705074273154, 35.64915139335016647 ) ) ;
#17387 = CARTESIAN_POINT ( 'NONE',  ( 43.01140435219951286, 104.6297705074273239, 29.55568802177586463 ) ) ;
#17388 = CARTESIAN_POINT ( 'NONE',  ( 19.13088699441526686, 95.37848931739559077, 15.19637875606281341 ) ) ;
#17389 = CARTESIAN_POINT ( 'NONE',  ( 43.01140435219951286, 132.8651871740940180, 38.86567161673127657 ) ) ;
#17390 = ADVANCED_FACE ( 'NONE', ( #12358, #16886 ), #465, .F. ) ;
#17391 = CARTESIAN_POINT ( 'NONE',  ( -154.5594255724347761, -189.0891397928654953, 40.14644641866476604 ) ) ;
#17392 = CARTESIAN_POINT ( 'NONE',  ( -142.0420953463936087, -165.6584106276440593, 49.65701158161630957 ) ) ;
#17393 = DIRECTION ( 'NONE',  ( 0.000000000000000000, 0.000000000000000000, 1.000000000000000000 ) ) ;
#17394 = EDGE_CURVE ( 'NONE', #137, #890, #17426, .T. ) ;
#17395 = CARTESIAN_POINT ( 'NONE',  ( 38.01140435219952707, 135.7104996726487514, 34.21067981925357060 ) ) ;
#17396 = CARTESIAN_POINT ( 'NONE',  ( 27.44638778410068625, 143.5188605762539851, 16.27111261720311930 ) ) ;
#17397 = LINE ( 'NONE', #12552, #18693 ) ;
#17398 = CARTESIAN_POINT ( 'NONE',  ( 38.58424406990784661, 117.2651871740940095, 35.64915139335016647 ) ) ;
#17399 = EDGE_CURVE ( 'NONE', #1684, #10985, #19693, .T. ) ;
#17400 = ORIENTED_EDGE ( 'NONE', *, *, #16785, .T. ) ;
#17401 = CARTESIAN_POINT ( 'NONE',  ( 156.7804311855217065, 208.8003142469820830, -44.99999999999997158 ) ) ;
#17402 = ORIENTED_EDGE ( 'NONE', *, *, #18688, .F. ) ;
#17403 = CARTESIAN_POINT ( 'NONE',  ( 38.01140435219952707, 89.78445800887257633, 34.21067981925357060 ) ) ;
#17404 = CARTESIAN_POINT ( 'NONE',  ( 40.27526882409969033, 60.82977050742731961, 37.97664729208901946 ) ) ;
#17406 = CARTESIAN_POINT ( 'NONE',  ( 57.63517438308760177, 95.88943085326536675, -6.196329169593343345 ) ) ;
#17405 = CARTESIAN_POINT ( 'NONE',  ( 41.64333658814960870, 117.7151871740939981, 38.42115945441014446 ) ) ;
#17407 = CARTESIAN_POINT ( 'NONE',  ( 39.92123440845004723, 70.16049967264873999, 38.46393386101376421 ) ) ;
#17409 = CARTESIAN_POINT ( 'NONE',  ( 48.01140435219951996, 136.4344580088725820, 32.58608133808903773 ) ) ;
#17408 = LINE ( 'NONE', #21771, #13276 ) ;
#17410 = CARTESIAN_POINT ( 'NONE',  ( -151.4692556286852891, -196.9891397928655010, 39.65701158161630246 ) ) ;
#17411 = CARTESIAN_POINT ( 'NONE',  ( -157.6495955161842062, -172.1130981290892805, 58.16351966513671812 ) ) ;
#17412 = CARTESIAN_POINT ( 'NONE',  ( 43.67008072911410466, 94.91368705836457309, 29.24343323619035928 ) ) ;
#17413 = CARTESIAN_POINT ( 'NONE',  ( 46.59305225739526435, 67.91518717409400097, 31.60846029578754468 ) ) ;
#17414 = DIRECTION ( 'NONE',  ( 0.000000000000000000, 0.000000000000000000, -1.000000000000000000 ) ) ;
#17415 = CARTESIAN_POINT ( 'NONE',  ( -157.2955611005346270, -184.4438272943107506, 57.67623309621198047 ) ) ;
#17416 = CARTESIAN_POINT ( 'NONE',  ( -151.4692556286852891, -191.9084106276440309, 39.74470866294723947 ) ) ;
#17417 = ORIENTED_EDGE ( 'NONE', *, *, #6596, .F. ) ;
#17418 = CARTESIAN_POINT ( 'NONE',  ( -159.0959885057557983, -175.8584106276440480, 55.19815736654470584 ) ) ;
#17419 = CARTESIAN_POINT ( 'NONE',  ( 47.97332496630577481, 153.8600623441721211, 10.00146007428102379 ) ) ;
#17420 = CARTESIAN_POINT ( 'NONE',  ( -151.4692556286852891, -182.3130981290892976, 39.65701158161629536 ) ) ;
#17421 = CARTESIAN_POINT ( 'NONE',  ( 45.74753988029933538, 148.1651871740940010, 37.97664729208901946 ) ) ;
#17422 = CARTESIAN_POINT ( 'NONE',  ( 47.43856463449117911, 106.7297705074273182, 35.64915139335015937 ) ) ;
#17423 = VERTEX_POINT ( 'NONE', #5078 ) ;
#17424 = ORIENTED_EDGE ( 'NONE', *, *, #7850, .T. ) ;
#17425 = CARTESIAN_POINT ( 'NONE',  ( 37.00104444766353851, 92.35499785847434850, 7.656504971210453370 ) ) ;
#17426 =( BOUNDED_CURVE ( )  B_SPLINE_CURVE ( 2, ( #15463, #144, #6875, #13582, #6987, #13690, #20425, #20533, #18768, #13796, #5420, #12580, #1007, #6173, #7743, #3994, #21178, #6069, #7633, #15775, #680, #5744, #10829, #17528, #15875, #789, #14337, #4306, #12796, #21077, #5959, #17745, #4409, #17855, #2766, #9382, #6060, #21504, #4623, #11343, #12787, #5949, #18066, #1105, #7840, #13119, #14542, #6162, #12897, #19617, #4512, #1212, #11235, #17955, #2973, #2860, #9603, #7945, #14651, #20284, #3310, #21615, #13225, #5073, #16634, #6625, #18297, #6740, #4847, #110, #698, #15095, #13447, #1545, #16518, #5287, #3427, #8164, #13340, #15210, #16849, #8276, #3531, #18517, #5179, #20182, #11787, #15320, #6506, #10147, #18180, #6842, #1764, #8386, #3086, #14976, #20077, #16958, #4965, #11568, #1434, #14870, #8498, #19963, #6950, #13548, #213, #8600, #11897, #3199, #18626, #13657, #9929, #10256, #20390, #11675, #21722, #1870, #9820, #18410, #10040, #16743, #1654, #755, #13976, #9144, #15431, #13762, #18839, #20502, #2088, #12107, #12324, #7384, #15844, #18734, #7490, #3852, #327, #7057, #5391, #3745, #3962, #10475, #20714, #5597, #12001, #9033, #17175, #8821, #14192, #20607, #15530, #4062, #2194, #10364, #10684, #20932, #8925, #12437, #435, #7166, #10577, #2408, #13869, #19163, #5490, #12217, #19059, #18951, #17280, #15630, #535, #7274, #15744, #17389, #2293, #649, #14085, #17065, #3639, #20821, #5712, #10791, #17497, #1978, #8712, #12981, #6138, #7920, #9470, #21258, #2944, #15951, #14518, #5813, #2835, #12870, #17818, #12544, #17710, #4596, #969, #14299, #10901, #11210, #2730, #14623, #18039, #19589, #4482, #21361, #19272, #4172, #6251, #7710, #12761, #9686, #2511, #11000, #16383, #16169, #19705, #11315, #14410, #1296, #21042, #8030, #17605, #1081, #14737, #21146, #9252, #12653, #17926, #2615, #862, #7599, #9574, #6031, #7812, #16280, #5925, #1186, #19377, #4272, #9353, #16058, #19482, #4373, #11104, #15181, #1738, #1518, #83, #8135, #11872, #21473, #11648, #8473, #14949, #6819, #18267, #8358, #13526, #10011, #14838, #20155, #6595, #16603, #5047, #5152, #11758, #16932, #10120, #18489, #20050, #11423, #1848, #13314, #3395, #6475, #21585, #11540, #13196, #21805, #16826, #3507, #6364, #18603, #4937, #3057, #16489, #1406, #19929, #20260, #10230, #8577, #4818, #18380, #13088, #3171, #9900, #19816, #8248, #21696, #4705, #3281, #18149, #9796, #16716, #1625, #15068, #6713, #13420, #17473, #1953, #17365, #411, #15606, #5262, #2166, #13737, #3719, #15406, #3827, #8683, #19034, #18924, #12189, #10553, #20475, #13629, #2383, #514, #11979, #10448, #12296, #13951, #20367, #8904, #7251, #2271, #17254, #20689, #12410, #3616, #5573, #15294, #3932, #10663, #5467, #187, #5367, #17150, #14061, #2066, #303, #18709, #9008, #15719, #17041, #4040, #623, #19141, #5687, #7358, #7032, #10338, #20795, #10767, #6924, #12084, #18814, #8795, #15509, #7142, #13845, #20581, #2700, #17792, #6007, #9551, #21017, #2813, #11292, #17580, #11187, #16029, #9445, #20903, #14492, #4571, #21123, #21234, #18014, #1163, #7687, #942, #7896, #6225, #7572, #7461, #9121, #16146, #5790, #19351, #6113, #7788, #14170, #1054, #17900, #15819, #12521, #5899, #12843, #19561, #4456, #16254, #14598, #11077, #12736, #733, #12629, #4249, #21338, #10975, #2486, #19247, #12956, #19459, #19679, #4146, #10879, #9228, #15926, #838, #14272, #17688, #2590, #14384, #9330, #4349, #18243, #21449, #14925, #18467, #5024, #4793, #3370, #11400, #15155, #2925, #6569, #11733, #3145, #16360, #9770, #1599, #14816, #55, #18123, #8332, #9875, #19905, #15041, #8449, #21782, #20237, #13396, #6689, #1494, #14713, #5129, #16575, #20130, #6339, #1714, #10094, #21561, #16801, #6797, #13504, #9660, #11848, #8224, #13065, #19792, #4684, #3033, #1271, #8006, #16467, #1381, #11514, #8110, #6451, #13174, #20025, #4910, #18354, #3258, #9988, #10207, #3483, #5544, #20448, #3692, #594, #15268, #1924, #15686, #7333, #5659, #274, #5340, #2142, #15381, #12057, #8875, #3909, #20663, #18789, #16910, #3586, #10528, #8659, #8980, #1823, #18893, #13712, #20558, #6898, #5443, #18576, #13605, #3800, #13924, #12271, #14033, #17226, #10419, #15582, #8556, #17339, #485, #7008, #19007, #7223, #166, #20342, #10635, #5237, #20768, #11954, #18684, #2246, #10315, #17016, #17124, #2036, #8768, #15483, #384, #7113, #13818, #8059, #16416, #14767, #2977, #16522, #6284, #21396, #1440, #11347, #1326, #18070, #12492, #4518, #3091, #1110, #13015, #2353, #9715, #8169, #2865, #21509, #21619, #4736, #11240, #17960, #11455, #9824, #6395, #2760, #16307, #13123, #6168, #19624, #19845, #18184, #10740, #19735, #14874, #12382, #9091, #9501, #19117, #4012, #17442, #4628, #15793, #14656, #702, #7436, #17850, #14139, #20876, #5764, #7845, #19219, #16198, #4117, #10853, #14547, #21290, #12902, #9608, #1217, #7951, #6631, #3431, #17068, #4852, #20394, #1982, #3, #3203, #18522, #217, #8603, #11901, #3315, #6744, #18630, #13660, #13452, #3641, #5290, #15323, #10044, #15215, #6953, #16853, #14981, #5182, #20186, #8390, #3534, #12004, #10259, #13553, #1873, #18738, #8715, #8502, #10367, #9934, #8280 ),
 .UNSPECIFIED., .F., .F. ) 
 B_SPLINE_CURVE_WITH_KNOTS ( ( 3, 2, 2, 2, 2, 2, 2, 2, 2, 2, 2, 2, 2, 2, 2, 2, 2, 2, 2, 2, 2, 2, 2, 2, 2, 2, 2, 2, 2, 2, 2, 2, 2, 2, 2, 2, 2, 2, 2, 2, 2, 2, 2, 2, 2, 2, 2, 2, 2, 2, 2, 2, 2, 2, 2, 2, 2, 2, 2, 2, 2, 2, 2, 2, 2, 2, 2, 2, 2, 2, 2, 2, 2, 2, 2, 2, 2, 2, 2, 2, 2, 2, 2, 2, 2, 2, 2, 2, 2, 2, 2, 2, 2, 2, 2, 2, 2, 2, 2, 2, 2, 2, 2, 2, 2, 2, 2, 2, 2, 2, 2, 2, 2, 2, 2, 2, 2, 2, 2, 2, 2, 2, 2, 2, 2, 2, 2, 2, 2, 2, 2, 2, 2, 2, 2, 2, 2, 2, 2, 2, 2, 2, 2, 2, 2, 2, 2, 2, 2, 2, 2, 2, 2, 2, 2, 2, 2, 2, 2, 2, 2, 2, 2, 2, 2, 2, 2, 2, 2, 2, 2, 2, 2, 2, 2, 2, 2, 2, 2, 2, 2, 2, 2, 2, 2, 2, 2, 2, 2, 2, 2, 2, 2, 2, 2, 2, 2, 2, 2, 2, 2, 2, 2, 2, 2, 2, 2, 2, 2, 2, 2, 2, 2, 2, 2, 2, 2, 2, 2, 2, 2, 2, 2, 2, 2, 2, 2, 2, 2, 2, 2, 2, 2, 2, 2, 2, 2, 2, 2, 2, 2, 2, 2, 2, 2, 2, 2, 2, 2, 2, 2, 2, 2, 2, 2, 2, 2, 2, 2, 2, 2, 2, 2, 2, 2, 2, 2, 2, 2, 2, 2, 2, 2, 2, 2, 2, 2, 2, 2, 2, 2, 2, 2, 2, 2, 2, 2, 2, 2, 2, 2, 2, 2, 2, 2, 2, 2, 2, 2, 2, 2, 2, 2, 2, 2, 2, 2, 2, 2, 2, 2, 2, 2, 2, 2, 2, 2, 2, 2, 2, 2, 2, 2, 2, 2, 2, 2, 2, 2, 2, 2, 2, 2, 2, 3 ),
 ( 0.000000000000000000, 0.002999988802223336245, 0.005999977604446672490, 0.008999966406670010036, 0.01199995520889334498, 0.01499994401111668166, 0.01799993281334002007, 0.02099992161556335502, 0.02399991041778668996, 0.02699989922001002837, 0.02999988802223336332, 0.03299987682445670173, 0.03599986562668004014, 0.03899985442890337856, 0.04199984323112671003, 0.04499983203335004844, 0.04799982083557337992, 0.05099980963779672527, 0.05399979844002005674, 0.05699978724224339516, 0.05999977604446672663, 0.06299976484669006505, 0.06599975364891340346, 0.06899974245113672799, 0.07199973125336008029, 0.07499972005558341870, 0.07799970885780675711, 0.08099969766003008165, 0.08399968646225342006, 0.08699967526447675847, 0.08999966406670009689, 0.09299965286892342142, 0.09599964167114675984, 0.09899963047337011213, 0.1019996192755934505, 0.1049996080778167751, 0.1079995968800401135, 0.1109995856822634519, 0.1139995744844867903, 0.1169995632867101149, 0.1199995520889334533, 0.1229995408911567917, 0.1259995296933801301, 0.1289995184956034546, 0.1319995072978268069, 0.1349994961000501315, 0.1379994849022734560, 0.1409994737044968360, 0.1439994625067201606, 0.1469994513089434851, 0.1499994401111668374, 0.1529994289133901619, 0.1559994177156135142, 0.1589994065178368388, 0.1619993953200601633, 0.1649993841222835156, 0.1679993729245068401, 0.1709993617267301647, 0.1739993505289535169, 0.1769993393311768415, 0.1799993281334001938, 0.1829993169356235183, 0.1859993057378468428, 0.1889992945400701951, 0.1919992833422935197, 0.1949992721445168442, 0.1979992609467402243, 0.2009992497489635488, 0.2039992385511869011, 0.2069992273534102256, 0.2099992161556335502, 0.2129992049578569024, 0.2159991937600802270, 0.2189991825623035515, 0.2219991713645269038, 0.2249991601667502283, 0.2279991489689735806, 0.2309991377711969052, 0.2339991265734202297, 0.2369991153756435820, 0.2399991041778669065, 0.2429990929800902311, 0.2459990817823135834, 0.2489990705845369079, 0.2519990593867602602, 0.2549990481889836125, 0.2579990369912069093, 0.2609990257934302615, 0.2639990145956536138, 0.2669990033978769661, 0.2699989922001002629, 0.2729989810023236152, 0.2759989698045469120, 0.2789989586067703198, 0.2819989474089936721, 0.2849989362112169689, 0.2879989250134403211, 0.2909989138156636179, 0.2939989026178869702, 0.2969988914201103225, 0.2999988802223336748, 0.3029988690245569716, 0.3059988578267803239, 0.3089988466290036206, 0.3119988354312270284, 0.3149988242334503252, 0.3179988130356736775, 0.3209988018378969743, 0.3239987906401203266, 0.3269987794423436789, 0.3299987682445670312, 0.3329987570467903280, 0.3359987458490136802, 0.3389987346512370325, 0.3419987234534603293, 0.3449987122556837371, 0.3479987010579070339, 0.3509986898601303862, 0.3539986786623536830, 0.3569986674645770353, 0.3599986562668003875, 0.3629986450690237398, 0.3659986338712470366, 0.3689986226734703889, 0.3719986114756936857, 0.3749986002779170935, 0.3779985890801403903, 0.3809985778823637426, 0.3839985666845870393, 0.3869985554868103916, 0.3899985442890336884, 0.3929985330912570962, 0.3959985218934804485, 0.3989985106957037453, 0.4019984994979270976, 0.4049984883001503944, 0.4079984771023738022, 0.4109984659045970989, 0.4139984547068204512, 0.4169984435090437480, 0.4199984323112671003, 0.4229984211134904526, 0.4259984099157138049, 0.4289983987179371017, 0.4319983875201604540, 0.4349983763223837507, 0.4379983651246071030, 0.4409983539268304553, 0.4439983427290538076, 0.4469983315312771044, 0.4499983203335004567, 0.4529983091357238090, 0.4559982979379471613, 0.4589982867401705136, 0.4619982755423938103, 0.4649982643446171626, 0.4679982531468404594, 0.4709982419490638672, 0.4739982307512871640, 0.4769982195535105163, 0.4799982083557338131, 0.4829981971579571653, 0.4859981859601804621, 0.4889981747624038699, 0.4919981635646271667, 0.4949981523668505190, 0.4979981411690738158, 0.5009981299712971126, 0.5039981187735205204, 0.5069981075757439282, 0.5099980963779672249, 0.5129980851801905217, 0.5159980739824138185, 0.5189980627846372263, 0.5219980515868605231, 0.5249980403890838199, 0.5279980291913072277, 0.5309980179935306355, 0.5339980067957539323, 0.5369979955979772290, 0.5399979844002005258, 0.5429979732024239336, 0.5459979620046472304, 0.5489979508068705272, 0.5519979396090938240, 0.5549979284113172318, 0.5579979172135406396, 0.5609979060157639363, 0.5639978948179873441, 0.5669978836202106409, 0.5699978724224339377, 0.5729978612246572345, 0.5759978500268806423, 0.5789978388291039391, 0.5819978276313272358, 0.5849978164335505326, 0.5879978052357739404, 0.5909977940379973482, 0.5939977828402206450, 0.5969977716424439418, 0.5999977604446673496, 0.6029977492468906464, 0.6059977380491139431, 0.6089977268513372399, 0.6119977156535606477, 0.6149977044557839445, 0.6179976932580072413, 0.6209976820602306491, 0.6239976708624540569, 0.6269976596646773537, 0.6299976484669006505, 0.6329976372691240583, 0.6359976260713473550, 0.6389976148735706518, 0.6419976036757939486, 0.6449975924780173564, 0.6479975812802406532, 0.6509975700824639500, 0.6539975588846873578, 0.6569975476869107656, 0.6599975364891340623, 0.6629975252913573591, 0.6659975140935806559, 0.6689975028958040637, 0.6719974916980273605, 0.6749974805002506573, 0.6779974693024740651, 0.6809974581046973618, 0.6839974469069206586, 0.6869974357091440664, 0.6899974245113674742, 0.6929974133135907710, 0.6959974021158140678, 0.6989973909180373646, 0.7019973797202607724, 0.7049973685224840692, 0.7079973573247073659, 0.7109973461269306627, 0.7139973349291540705, 0.7169973237313773673, 0.7199973125336007751, 0.7229973013358240719, 0.7259972901380474797, 0.7289972789402707765, 0.7319972677424940732, 0.7349972565447174810, 0.7379972453469407778, 0.7409972341491640746, 0.7439972229513873714, 0.7469972117536107792, 0.7499972005558341870, 0.7529971893580574838, 0.7559971781602807805, 0.7589971669625041883, 0.7619971557647274851, 0.7649971445669507819, 0.7679971333691740787, 0.7709971221713974865, 0.7739971109736207833, 0.7769970997758440800, 0.7799970885780673768, 0.7829970773802908957, 0.7859970661825141924, 0.7889970549847374892, 0.7919970437869608970, 0.7949970325891841938, 0.7979970213914074906, 0.8009970101936307874, 0.8039969989958541952, 0.8069969877980774919, 0.8099969766003007887, 0.8129969654025241965, 0.8159969542047476043, 0.8189969430069709011, 0.8219969318091941979, 0.8249969206114174947, 0.8279969094136409025, 0.8309968982158641992, 0.8339968870180874960, 0.8369968758203107928, 0.8399968646225342006, 0.8429968534247574974, 0.8459968422269809052, 0.8489968310292043130, 0.8519968198314276098, 0.8549968086336509066, 0.8579967974358742033, 0.8609967862380976111, 0.8639967750403209079, 0.8669967638425442047, 0.8699967526447675015, 0.8729967414469909093, 0.8759967302492142061, 0.8789967190514376139, 0.8819967078536609106, 0.8849966966558843184, 0.8879966854581076152, 0.8909966742603309120, 0.8939966630625542088, 0.8969966518647776166, 0.8999966406670009134, 0.9029966294692242101, 0.9059966182714476179, 0.9089966070736710257, 0.9119965958758943225, 0.9149965846781176193, 0.9179965734803410271, 0.9209965622825643239, 0.9239965510847876207, 0.9269965398870109174, 0.9299965286892343252, 0.9329965174914576220, 0.9359965062936809188, 0.9389964950959042156, 0.9419964838981277344, 0.9449964727003510312, 0.9479964615025743280, 0.9509964503047977358, 0.9539964391070210326, 0.9569964279092443293, 0.9599964167114676261, 0.9629964055136910339, 0.9659963943159143307, 0.9689963831181376275, 0.9719963719203609243, 0.9749963607225844431, 0.9779963495248077399, 0.9809963383270310366, 0.9839963271292543334, 0.9869963159314777412, 0.9899963047337010380, 0.9929962935359243348, 0.9959962823381476316, 0.9989962711403710394, 1.000000000000000000 ),
 .UNSPECIFIED. ) 
 CURVE ( )  GEOMETRIC_REPRESENTATION_ITEM ( )  RATIONAL_B_SPLINE_CURVE ( ( 1.000000000000000000, 0.9510565162951535312, 1.000000000000000000, 0.9510565162951535312, 1.000000000000000000, 0.9510565162951535312, 1.000000000000000000, 0.9510565162951535312, 1.000000000000000000, 0.9510565162951535312, 1.000000000000000000, 0.9510565162951535312, 1.000000000000000000, 0.9510565162951535312, 1.000000000000000000, 0.9510565162951535312, 1.000000000000000000, 0.9510565162951535312, 1.000000000000000000, 0.9510565162951535312, 1.000000000000000000, 0.9510565162951535312, 1.000000000000000000, 0.9510565162951535312, 1.000000000000000000, 0.9510565162951535312, 1.000000000000000000, 0.9510565162951535312, 1.000000000000000000, 0.9510565162951535312, 1.000000000000000000, 0.9510565162951535312, 1.000000000000000000, 0.9510565162951535312, 1.000000000000000000, 0.9510565162951535312, 1.000000000000000000, 0.9510565162951535312, 1.000000000000000000, 0.9510565162951535312, 1.000000000000000000, 0.9510565162951535312, 1.000000000000000000, 0.9510565162951535312, 1.000000000000000000, 0.9510565162951535312, 1.000000000000000000, 0.9510565162951535312, 1.000000000000000000, 0.9510565162951535312, 1.000000000000000000, 0.9510565162951535312, 1.000000000000000000, 0.9510565162951535312, 1.000000000000000000, 0.9510565162951535312, 1.000000000000000000, 0.9510565162951535312, 1.000000000000000000, 0.9510565162951535312, 1.000000000000000000, 0.9510565162951535312, 1.000000000000000000, 0.9510565162951535312, 1.000000000000000000, 0.9510565162951535312, 1.000000000000000000, 0.9510565162951535312, 1.000000000000000000, 0.9510565162951535312, 1.000000000000000000, 0.9510565162951535312, 1.000000000000000000, 0.9510565162951535312, 1.000000000000000000, 0.9510565162951535312, 1.000000000000000000, 0.9510565162951535312, 1.000000000000000000, 0.9510565162951535312, 1.000000000000000000, 0.9510565162951535312, 1.000000000000000000, 0.9510565162951535312, 1.000000000000000000, 0.9510565162951535312, 1.000000000000000000, 0.9510565162951535312, 1.000000000000000000, 0.9510565162951535312, 1.000000000000000000, 0.9510565162951535312, 1.000000000000000000, 0.9510565162951535312, 1.000000000000000000, 0.9510565162951535312, 1.000000000000000000, 0.9510565162951535312, 1.000000000000000000, 0.9510565162951535312, 1.000000000000000000, 0.9510565162951535312, 1.000000000000000000, 0.9510565162951535312, 1.000000000000000000, 0.9510565162951535312, 1.000000000000000000, 0.9510565162951535312, 1.000000000000000000, 0.9510565162951535312, 1.000000000000000000, 0.9510565162951535312, 1.000000000000000000, 0.9510565162951535312, 1.000000000000000000, 0.9510565162951535312, 1.000000000000000000, 0.9510565162951535312, 1.000000000000000000, 0.9510565162951535312, 1.000000000000000000, 0.9510565162951535312, 1.000000000000000000, 0.9510565162951535312, 1.000000000000000000, 0.9510565162951535312, 1.000000000000000000, 0.9510565162951535312, 1.000000000000000000, 0.9510565162951535312, 1.000000000000000000, 0.9510565162951535312, 1.000000000000000000, 0.9510565162951535312, 1.000000000000000000, 0.9510565162951535312, 1.000000000000000000, 0.9510565162951535312, 1.000000000000000000, 0.9510565162951535312, 1.000000000000000000, 0.9510565162951535312, 1.000000000000000000, 0.9510565162951535312, 1.000000000000000000, 0.9510565162951535312, 1.000000000000000000, 0.9510565162951535312, 1.000000000000000000, 0.9510565162951535312, 1.000000000000000000, 0.9510565162951535312, 1.000000000000000000, 0.9510565162951535312, 1.000000000000000000, 0.9510565162951535312, 1.000000000000000000, 0.9510565162951535312, 1.000000000000000000, 0.9510565162951535312, 1.000000000000000000, 0.9510565162951535312, 1.000000000000000000, 0.9510565162951535312, 1.000000000000000000, 0.9510565162951535312, 1.000000000000000000, 0.9510565162951535312, 1.000000000000000000, 0.9510565162951535312, 1.000000000000000000, 0.9510565162951535312, 1.000000000000000000, 0.9510565162951535312, 1.000000000000000000, 0.9510565162951535312, 1.000000000000000000, 0.9510565162951535312, 1.000000000000000000, 0.9510565162951535312, 1.000000000000000000, 0.9510565162951535312, 1.000000000000000000, 0.9510565162951535312, 1.000000000000000000, 0.9510565162951535312, 1.000000000000000000, 0.9510565162951535312, 1.000000000000000000, 0.9510565162951535312, 1.000000000000000000, 0.9510565162951535312, 1.000000000000000000, 0.9510565162951535312, 1.000000000000000000, 0.9510565162951535312, 1.000000000000000000, 0.9510565162951535312, 1.000000000000000000, 0.9510565162951535312, 1.000000000000000000, 0.9510565162951535312, 1.000000000000000000, 0.9510565162951535312, 1.000000000000000000, 0.9510565162951535312, 1.000000000000000000, 0.9510565162951535312, 1.000000000000000000, 0.9510565162951535312, 1.000000000000000000, 0.9510565162951535312, 1.000000000000000000, 0.9510565162951535312, 1.000000000000000000, 0.9510565162951535312, 1.000000000000000000, 0.9510565162951535312, 1.000000000000000000, 0.9510565162951535312, 1.000000000000000000, 0.9510565162951535312, 1.000000000000000000, 0.9510565162951535312, 1.000000000000000000, 0.9510565162951535312, 1.000000000000000000, 0.9510565162951535312, 1.000000000000000000, 0.9510565162951535312, 1.000000000000000000, 0.9510565162951535312, 1.000000000000000000, 0.9510565162951535312, 1.000000000000000000, 0.9510565162951535312, 1.000000000000000000, 0.9510565162951535312, 1.000000000000000000, 0.9510565162951535312, 1.000000000000000000, 0.9510565162951535312, 1.000000000000000000, 0.9510565162951535312, 1.000000000000000000, 0.9510565162951535312, 1.000000000000000000, 0.9510565162951535312, 1.000000000000000000, 0.9510565162951535312, 1.000000000000000000, 0.9510565162951535312, 1.000000000000000000, 0.9510565162951535312, 1.000000000000000000, 0.9510565162951535312, 1.000000000000000000, 0.9510565162951535312, 1.000000000000000000, 0.9510565162951535312, 1.000000000000000000, 0.9510565162951535312, 1.000000000000000000, 0.9510565162951535312, 1.000000000000000000, 0.9510565162951535312, 1.000000000000000000, 0.9510565162951535312, 1.000000000000000000, 0.9510565162951535312, 1.000000000000000000, 0.9510565162951535312, 1.000000000000000000, 0.9510565162951535312, 1.000000000000000000, 0.9510565162951535312, 1.000000000000000000, 0.9510565162951535312, 1.000000000000000000, 0.9510565162951535312, 1.000000000000000000, 0.9510565162951535312, 1.000000000000000000, 0.9510565162951535312, 1.000000000000000000, 0.9510565162951535312, 1.000000000000000000, 0.9510565162951535312, 1.000000000000000000, 0.9510565162951535312, 1.000000000000000000, 0.9510565162951535312, 1.000000000000000000, 0.9510565162951535312, 1.000000000000000000, 0.9510565162951535312, 1.000000000000000000, 0.9510565162951535312, 1.000000000000000000, 0.9510565162951535312, 1.000000000000000000, 0.9510565162951535312, 1.000000000000000000, 0.9510565162951535312, 1.000000000000000000, 0.9510565162951535312, 1.000000000000000000, 0.9510565162951535312, 1.000000000000000000, 0.9510565162951535312, 1.000000000000000000, 0.9510565162951535312, 1.000000000000000000, 0.9510565162951535312, 1.000000000000000000, 0.9510565162951535312, 1.000000000000000000, 0.9510565162951535312, 1.000000000000000000, 0.9510565162951535312, 1.000000000000000000, 0.9510565162951535312, 1.000000000000000000, 0.9510565162951535312, 1.000000000000000000, 0.9510565162951535312, 1.000000000000000000, 0.9510565162951535312, 1.000000000000000000, 0.9510565162951535312, 1.000000000000000000, 0.9510565162951535312, 1.000000000000000000, 0.9510565162951535312, 1.000000000000000000, 0.9510565162951535312, 1.000000000000000000, 0.9510565162951535312, 1.000000000000000000, 0.9510565162951535312, 1.000000000000000000, 0.9510565162951535312, 1.000000000000000000, 0.9510565162951535312, 1.000000000000000000, 0.9510565162951535312, 1.000000000000000000, 0.9510565162951535312, 1.000000000000000000, 0.9510565162951535312, 1.000000000000000000, 0.9510565162951535312, 1.000000000000000000, 0.9510565162951535312, 1.000000000000000000, 0.9510565162951535312, 1.000000000000000000, 0.9510565162951535312, 1.000000000000000000, 0.9510565162951535312, 1.000000000000000000, 0.9510565162951535312, 1.000000000000000000, 0.9510565162951535312, 1.000000000000000000, 0.9510565162951535312, 1.000000000000000000, 0.9510565162951535312, 1.000000000000000000, 0.9510565162951535312, 1.000000000000000000, 0.9510565162951535312, 1.000000000000000000, 0.9510565162951535312, 1.000000000000000000, 0.9510565162951535312, 1.000000000000000000, 0.9510565162951535312, 1.000000000000000000, 0.9510565162951535312, 1.000000000000000000, 0.9510565162951535312, 1.000000000000000000, 0.9510565162951535312, 1.000000000000000000, 0.9510565162951535312, 1.000000000000000000, 0.9510565162951535312, 1.000000000000000000, 0.9510565162951535312, 1.000000000000000000, 0.9510565162951535312, 1.000000000000000000, 0.9510565162951535312, 1.000000000000000000, 0.9510565162951535312, 1.000000000000000000, 0.9510565162951535312, 1.000000000000000000, 0.9510565162951535312, 1.000000000000000000, 0.9510565162951535312, 1.000000000000000000, 0.9510565162951535312, 1.000000000000000000, 0.9510565162951535312, 1.000000000000000000, 0.9510565162951535312, 1.000000000000000000, 0.9510565162951535312, 1.000000000000000000, 0.9510565162951535312, 1.000000000000000000, 0.9510565162951535312, 1.000000000000000000, 0.9510565162951535312, 1.000000000000000000, 0.9510565162951535312, 1.000000000000000000, 0.9510565162951535312, 1.000000000000000000, 0.9510565162951535312, 1.000000000000000000, 0.9510565162951535312, 1.000000000000000000, 0.9510565162951535312, 1.000000000000000000, 0.9510565162951535312, 1.000000000000000000, 0.9510565162951535312, 1.000000000000000000, 0.9510565162951535312, 1.000000000000000000, 0.9510565162951535312, 1.000000000000000000, 0.9510565162951535312, 1.000000000000000000, 0.9510565162951535312, 1.000000000000000000, 0.9510565162951535312, 1.000000000000000000, 0.9510565162951535312, 1.000000000000000000, 0.9510565162951535312, 1.000000000000000000, 0.9510565162951535312, 1.000000000000000000, 0.9510565162951535312, 1.000000000000000000, 0.9510565162951535312, 1.000000000000000000, 0.9510565162951535312, 1.000000000000000000, 0.9510565162951535312, 1.000000000000000000, 0.9510565162951535312, 1.000000000000000000, 0.9510565162951535312, 1.000000000000000000, 0.9510565162951535312, 1.000000000000000000, 0.9510565162951535312, 1.000000000000000000, 0.9510565162951535312, 1.000000000000000000, 0.9510565162951535312, 1.000000000000000000, 0.9510565162951535312, 1.000000000000000000, 0.9510565162951535312, 1.000000000000000000, 0.9510565162951535312, 1.000000000000000000, 0.9510565162951535312, 1.000000000000000000, 0.9510565162951535312, 1.000000000000000000, 0.9510565162951535312, 1.000000000000000000, 0.9510565162951535312, 1.000000000000000000, 0.9510565162951535312, 1.000000000000000000, 0.9510565162951535312, 1.000000000000000000, 0.9510565162951535312, 1.000000000000000000, 0.9510565162951535312, 1.000000000000000000, 0.9510565162951535312, 1.000000000000000000, 0.9510565162951535312, 1.000000000000000000, 0.9510565162951535312, 1.000000000000000000, 0.9510565162951535312, 1.000000000000000000, 0.9510565162951535312, 1.000000000000000000, 0.9510565162951535312, 1.000000000000000000, 0.9510565162951535312, 1.000000000000000000, 0.9510565162951535312, 1.000000000000000000, 0.9510565162951535312, 1.000000000000000000, 0.9510565162951535312, 1.000000000000000000, 0.9510565162951535312, 1.000000000000000000, 0.9510565162951535312, 1.000000000000000000, 0.9510565162951535312, 1.000000000000000000, 0.9510565162951535312, 1.000000000000000000, 0.9510565162951535312, 1.000000000000000000, 0.9510565162951535312, 1.000000000000000000, 0.9510565162951535312, 1.000000000000000000, 0.9510565162951535312, 1.000000000000000000, 0.9510565162951535312, 1.000000000000000000, 0.9510565162951535312, 1.000000000000000000, 0.9510565162951535312, 1.000000000000000000, 0.9510565162951535312, 1.000000000000000000, 0.9510565162951535312, 1.000000000000000000, 0.9510565162951535312, 1.000000000000000000, 0.9510565162951535312, 1.000000000000000000, 0.9510565162951535312, 1.000000000000000000, 0.9510565162951535312, 1.000000000000000000, 0.9510565162951535312, 1.000000000000000000, 0.9510565162951535312, 1.000000000000000000, 0.9510565162951535312, 1.000000000000000000, 0.9510565162951535312, 1.000000000000000000, 0.9510565162951535312, 1.000000000000000000, 0.9510565162951535312, 1.000000000000000000, 0.9510565162951535312, 1.000000000000000000, 0.9510565162951535312, 1.000000000000000000, 0.9510565162951535312, 1.000000000000000000, 0.9510565162951535312, 1.000000000000000000, 0.9510565162951535312, 1.000000000000000000, 0.9510565162951535312, 1.000000000000000000, 0.9510565162951535312, 1.000000000000000000, 0.9510565162951535312, 1.000000000000000000, 0.9510565162951535312, 1.000000000000000000, 0.9510565162951535312, 1.000000000000000000, 0.9510565162951535312, 1.000000000000000000, 0.9510565162951535312, 1.000000000000000000, 0.9510565162951535312, 1.000000000000000000, 0.9510565162951535312, 1.000000000000000000, 0.9510565162951535312, 1.000000000000000000, 0.9510565162951535312, 1.000000000000000000, 0.9510565162951535312, 1.000000000000000000, 0.9510565162951535312, 1.000000000000000000, 0.9510565162951535312, 1.000000000000000000, 0.9510565162951535312, 1.000000000000000000, 0.9510565162951535312, 1.000000000000000000, 0.9510565162951535312, 1.000000000000000000, 0.9510565162951535312, 1.000000000000000000, 0.9510565162951535312, 1.000000000000000000, 0.9510565162951535312, 1.000000000000000000, 0.9510565162951535312, 1.000000000000000000, 0.9510565162951535312, 1.000000000000000000, 0.9510565162951535312, 1.000000000000000000, 0.9510565162951535312, 1.000000000000000000, 0.9510565162951535312, 1.000000000000000000, 0.9510565162951535312, 1.000000000000000000, 0.9510565162951535312, 1.000000000000000000, 0.9510565162951535312, 1.000000000000000000, 0.9510565162951535312, 1.000000000000000000, 0.9510565162951535312, 1.000000000000000000, 0.9510565162951535312, 1.000000000000000000, 0.9510565162951535312, 1.000000000000000000, 0.9510565162951535312, 1.000000000000000000, 0.9510565162951535312, 1.000000000000000000, 0.9510565162951535312, 1.000000000000000000, 0.9510565162951535312, 1.000000000000000000, 0.9510565162951535312, 1.000000000000000000, 0.9510565162951535312, 1.000000000000000000, 0.9510565162951535312, 1.000000000000000000, 0.9510565162951535312, 1.000000000000000000, 0.9510565162951535312, 1.000000000000000000, 0.9510565162951535312, 1.000000000000000000, 0.9510565162951535312, 1.000000000000000000, 0.9510565162951535312, 1.000000000000000000, 0.9510565162951535312, 1.000000000000000000, 0.9510565162951535312, 1.000000000000000000, 0.9510565162951535312, 1.000000000000000000, 0.9510565162951535312, 1.000000000000000000, 0.9510565162951535312, 1.000000000000000000, 0.9510565162951535312, 1.000000000000000000, 0.9510565162951535312, 1.000000000000000000, 0.9836246098489007661, 0.9782068950532306628 ) ) 
 REPRESENTATION_ITEM ( '' )  );
#17427 = VERTEX_POINT ( 'NONE', #11680 ) ;
#17428 = EDGE_CURVE ( 'NONE', #16883, #10216, #18416, .T. ) ;
#17429 = CARTESIAN_POINT ( 'NONE',  ( 39.92123440845005433, 76.16049967264873999, 38.46393386101375711 ) ) ;
#17430 = VECTOR ( 'NONE', #14176, 1000.000000000000000 ) ;
#17431 = CARTESIAN_POINT ( 'NONE',  ( 43.01140435219951286, 144.8651871740939612, 38.86567161673127657 ) ) ;
#17432 = CARTESIAN_POINT ( 'NONE',  ( 39.92123440845004723, 100.1604996726487116, 38.46393386101376421 ) ) ;
#17433 = CARTESIAN_POINT ( 'NONE',  ( 13.33420504782278293, 102.8437529505761603, 1.505736668420971869 ) ) ;
#17434 = CARTESIAN_POINT ( 'NONE',  ( 125.6223472235027998, 193.0332408774651185, 4.000000000000021316 ) ) ;
#17435 = CARTESIAN_POINT ( 'NONE',  ( -159.5594255724347761, -170.7891397928654840, 43.77915905869157598 ) ) ;
#17436 = CARTESIAN_POINT ( 'NONE',  ( 43.01140435219951996, 10.71049967264875491, 39.21067981925356349 ) ) ;
#17437 = CARTESIAN_POINT ( 'NONE',  ( 41.46631938032478359, 143.1844580088725820, 29.45539723777780239 ) ) ;
#17438 = CARTESIAN_POINT ( 'NONE',  ( -161.4692556286853176, -163.5630981290893260, 49.65701158161630957 ) ) ;
#17439 = ORIENTED_EDGE ( 'NONE', *, *, #13663, .F. ) ;
#17440 = CARTESIAN_POINT ( 'NONE',  ( 43.01140435219951286, 89.62977050742729546, 29.55568802177586463 ) ) ;
#17441 = CARTESIAN_POINT ( 'NONE',  ( -143.8425227516148084, -168.0938272943107563, 44.11586579668791330 ) ) ;
#17442 = CARTESIAN_POINT ( 'NONE',  ( 47.43856463449117911, 67.76518717409399528, 32.77220824515697473 ) ) ;
#17443 = CARTESIAN_POINT ( 'NONE',  ( 53.88337135589062399, 152.3674195137575964, -9.803719146365084569 ) ) ;
#17444 = DIRECTION ( 'NONE',  ( 0.9385982292947087080, 0.3450121214752279730, 0.000000000000000000 ) ) ;
#17445 = VECTOR ( 'NONE', #9951, 1000.000000000000000 ) ;
#17446 = EDGE_LOOP ( 'NONE', ( #9183, #11929, #6075, #13927 ) ) ;
#17447 = EDGE_CURVE ( 'NONE', #784, #1116, #11792, .T. ) ;
#17448 = CARTESIAN_POINT ( 'NONE',  ( 39.92123440845005433, 117.2604996726487485, 29.95742577749336988 ) ) ;
#17449 = DIRECTION ( 'NONE',  ( 0.000000000000000000, 0.000000000000000000, 1.000000000000000000 ) ) ;
#17450 = CARTESIAN_POINT ( 'NONE',  ( 44.37947211624943833, 134.4797705074273324, 30.00020018409699318 ) ) ;
#17451 = CARTESIAN_POINT ( 'NONE',  ( 14.94553207812311690, 121.6546367895698779, 10.23235069918434981 ) ) ;
#17452 = EDGE_LOOP ( 'NONE', ( #2551, #19766, #20400, #9780 ) ) ;
#17453 = CYLINDRICAL_SURFACE ( 'NONE', #14666, 7.500000000000007105 ) ;
#17454 = VERTEX_POINT ( 'NONE', #6845 ) ;
#17455 = CARTESIAN_POINT ( 'NONE',  ( 47.43856463449117200, 140.0297705074273438, 32.77220824515698183 ) ) ;
#17456 = CARTESIAN_POINT ( 'NONE',  ( 48.01140435219951996, 139.2844580088725763, 34.21067981925357060 ) ) ;
#17457 = AXIS2_PLACEMENT_3D ( 'NONE', #6383, #4725, #18171 ) ;
#17458 = CARTESIAN_POINT ( 'NONE',  ( 38.01140435219952707, 99.71049967264875136, 34.21067981925357060 ) ) ;
#17459 = DIRECTION ( 'NONE',  ( 1.000000000000000000, 0.000000000000000000, 0.000000000000000000 ) ) ;
#17460 = SURFACE_SIDE_STYLE ('',( #12510 ) ) ;
#17461 = VECTOR ( 'NONE', #21544, 999.9999999999998863 ) ;
#17462 = CARTESIAN_POINT ( 'NONE',  ( 43.01140435219951286, 95.36518717409400381, 29.55568802177586463 ) ) ;
#17463 = CARTESIAN_POINT ( 'NONE',  ( 38.01140435219952707, 66.71049967264873715, 34.21067981925357060 ) ) ;
#17464 = CARTESIAN_POINT ( 'NONE',  ( 136.2707191487307341, 181.8577005505615034, 22.21145758847113427 ) ) ;
#17465 = CARTESIAN_POINT ( 'NONE',  ( -143.3790856849358306, -155.7630981290893146, 43.77915905869157598 ) ) ;
#17466 = CARTESIAN_POINT ( 'NONE',  ( 0.000000000000000000, 0.000000000000000000, 0.000000000000000000 ) ) ;
#17467 = CARTESIAN_POINT ( 'NONE',  ( 47.05648932407426344, 70.91049967264873999, 37.14960608071593384 ) ) ;
#17468 = SHAPE_REPRESENTATION ( 'Handle Grip', ( #12657 ), #11603 ) ;
#17469 = CARTESIAN_POINT ( 'NONE',  ( 41.46631938032478359, 134.1844580088725820, 29.45539723777780239 ) ) ;
#17470 = CARTESIAN_POINT ( 'NONE',  ( 38.58424406990784661, 114.5297705074273296, 35.64915139335016647 ) ) ;
#17471 = CARTESIAN_POINT ( 'NONE',  ( 69.40534582624466964, 109.7482951092767678, 5.080680574306066788 ) ) ;
#17472 = DIRECTION ( 'NONE',  ( 0.000000000000000000, 0.000000000000000000, 1.000000000000000000 ) ) ;
#17473 = CARTESIAN_POINT ( 'NONE',  ( 43.01140435219951286, 111.8651871740939896, 38.86567161673127657 ) ) ;
#17474 = DIRECTION ( 'NONE',  ( 1.000000000000000000, 0.000000000000000000, 0.000000000000000000 ) ) ;
#17475 = ORIENTED_EDGE ( 'NONE', *, *, #3646, .F. ) ;
#17476 = EDGE_CURVE ( 'NONE', #2417, #7018, #20288, .T. ) ;
#17477 = CARTESIAN_POINT ( 'NONE',  ( 48.01140435219951996, 157.4344580088725820, 32.58608133808903773 ) ) ;
#17478 = CARTESIAN_POINT ( 'NONE',  ( 31.29766364123476663, 87.82482650329993135, 8.724447585906515812 ) ) ;
#17479 = AXIS2_PLACEMENT_3D ( 'NONE', #6810, #11861, #8568 ) ;
#17480 = CARTESIAN_POINT ( 'NONE',  ( 14.88799800344823154, 117.8296896831652560, 9.085076399755989129 ) ) ;
#17481 = DIRECTION ( 'NONE',  ( 0.000000000000000000, 0.000000000000000000, 1.000000000000000000 ) ) ;
#17482 = CARTESIAN_POINT ( 'NONE',  ( 46.59305225739526435, 73.57977050742732672, 36.81289934271958941 ) ) ;
#17483 = ORIENTED_EDGE ( 'NONE', *, *, #1543, .T. ) ;
#17484 = ORIENTED_EDGE ( 'NONE', *, *, #14513, .T. ) ;
#17485 = CARTESIAN_POINT ( 'NONE',  ( -145.2889157411863437, -165.5130981290892862, 58.16351966513671812 ) ) ;
#17486 = CARTESIAN_POINT ( 'NONE',  ( 48.01140435219951996, 119.2104996726487371, 34.21067981925357060 ) ) ;
#17488 = CARTESIAN_POINT ( 'NONE',  ( 76.67641731516037851, 114.1545672503790740, -7.227887495354823777 ) ) ;
#17487 = CARTESIAN_POINT ( 'NONE',  ( 38.58424406990784661, 81.26518717409398107, 35.64915139335016647 ) ) ;
#17489 = AXIS2_PLACEMENT_3D ( 'NONE', #9374, #2424, #19184 ) ;
#17490 = CARTESIAN_POINT ( 'NONE',  ( -157.2955611005345986, -170.3438272943107563, 41.63779006702063867 ) ) ;
#17491 = CARTESIAN_POINT ( 'NONE',  ( 8.829984022807513711, 121.7968051057545580, 16.14860047415989541 ) ) ;
#17492 = CARTESIAN_POINT ( 'NONE',  ( -161.4692556286852607, -190.4130981290892919, 52.90620854394536821 ) ) ;
#17493 = DIRECTION ( 'NONE',  ( 0.000000000000000000, 0.000000000000000000, 1.000000000000000000 ) ) ;
#17494 = CARTESIAN_POINT ( 'NONE',  ( 39.92123440845005433, 149.3344580088725593, 29.95742577749336988 ) ) ;
#17495 = CARTESIAN_POINT ( 'NONE',  ( 43.01140435219951286, 139.1297705074272812, 38.86567161673127657 ) ) ;
#17496 = CARTESIAN_POINT ( 'NONE',  ( 36.57762280775352082, 86.20069522707665044, 6.548861720777491513 ) ) ;
#17497 = CARTESIAN_POINT ( 'NONE',  ( 41.64333658814960870, 131.5151871740939953, 30.00020018409699318 ) ) ;
#17498 = CARTESIAN_POINT ( 'NONE',  ( -159.0959885057557983, -164.4584106276440423, 44.11586579668791330 ) ) ;
#17499 = CARTESIAN_POINT ( 'NONE',  ( -157.6495955161842062, -164.0391397928654555, 58.16351966513671812 ) ) ;
#17500 = CARTESIAN_POINT ( 'NONE',  ( 48.01140435219951996, 91.43445800887258201, 32.58608133808903773 ) ) ;
#17501 = CARTESIAN_POINT ( 'NONE',  ( 71.27174135432656499, 120.9783100490299574, 11.62814500561148456 ) ) ;
#17502 = VECTOR ( 'NONE', #6454, 1000.000000000000000 ) ;
#17503 = CARTESIAN_POINT ( 'NONE',  ( 141.4773229304660447, 84.89323405393692212, 4.000000000000021316 ) ) ;
#17504 = CARTESIAN_POINT ( 'NONE',  ( 46.59305225739526435, 112.9151871740940010, 31.60846029578754468 ) ) ;
#17505 = ORIENTED_EDGE ( 'NONE', *, *, #13847, .F. ) ;
#17506 = VECTOR ( 'NONE', #3026, 1000.000000000000000 ) ;
#17507 = CARTESIAN_POINT ( 'NONE',  ( -151.4692556286852607, -159.8130981290892692, 59.65701158161632378 ) ) ;
#17508 = EDGE_LOOP ( 'NONE', ( #21644, #17234 ) ) ;
#17509 = CARTESIAN_POINT ( 'NONE',  ( 43.01140435219951286, 87.53445800887256212, 39.46799094044489209 ) ) ;
#17510 = CARTESIAN_POINT ( 'NONE',  ( 43.01140435219951286, 151.1297705074273097, 38.86567161673127657 ) ) ;
#17511 = CARTESIAN_POINT ( 'NONE',  ( 39.92123440845004723, 147.2604996726487059, 29.95742577749337343 ) ) ;
#17513 = CARTESIAN_POINT ( 'NONE',  ( 71.07673676950255981, 118.1590465568689581, -7.267641430287227422 ) ) ;
#17512 = CARTESIAN_POINT ( 'NONE',  ( 41.64333658814960870, 107.5151871740939953, 30.00020018409699318 ) ) ;
#17514 = CARTESIAN_POINT ( 'NONE',  ( 48.01140435219951996, 74.21049967264873715, 34.21067981925357060 ) ) ;
#17516 = CARTESIAN_POINT ( 'NONE',  ( 47.05648932407426344, 61.58445800887258059, 31.27175355779120025 ) ) ;
#17515 = DIRECTION ( 'NONE',  ( 0.9387810623359077455, 0.3426822732243072211, 0.03548206049944095664 ) ) ;
#17517 = CARTESIAN_POINT ( 'NONE',  ( 43.01140435219951286, 72.53445800887256212, 39.21067981925356349 ) ) ;
#17518 = CARTESIAN_POINT ( 'NONE',  ( -157.6495955161842062, -190.1130981290892805, 58.16351966513671812 ) ) ;
#17519 = CARTESIAN_POINT ( 'NONE',  ( 41.64333658814960870, 66.71518717409399812, 38.42115945441014446 ) ) ;
#17520 = CIRCLE ( 'NONE', #1342, 27.14138364107347812 ) ;
#17521 = CARTESIAN_POINT ( 'NONE',  ( 38.01140435219952707, 63.86049967264874283, 35.83527830041809636 ) ) ;
#17522 = CARTESIAN_POINT ( 'NONE',  ( -148.5561028927606344, -177.9938272943107336, 58.62277379824867296 ) ) ;
#17523 = VERTEX_POINT ( 'NONE', #20936 ) ;
#17524 = CARTESIAN_POINT ( 'NONE',  ( -142.0420953463935803, -174.5084106276440252, 46.59394152635518793 ) ) ;
#17525 = CARTESIAN_POINT ( 'NONE',  ( 17.69433683334896656, 96.74512228834443306, 7.263443568815639573 ) ) ;
#17526 = ORIENTED_EDGE ( 'NONE', *, *, #1386, .F. ) ;
#17527 = CARTESIAN_POINT ( 'NONE',  ( 41.64333658814960870, 146.5151871740939953, 30.00020018409699318 ) ) ;
#17528 = CARTESIAN_POINT ( 'NONE',  ( 40.27526882409969744, 155.6651871740940010, 30.44471234641812174 ) ) ;
#17529 = CARTESIAN_POINT ( 'NONE',  ( 38.58424406990785371, 105.2297705074273040, 32.77220824515697473 ) ) ;
#17530 = ORIENTED_EDGE ( 'NONE', *, *, #17350, .T. ) ;
#17531 = ORIENTED_EDGE ( 'NONE', *, *, #13725, .F. ) ;
#17532 = CARTESIAN_POINT ( 'NONE',  ( 45.98873144221455789, 91.86516812052268222, 7.299390993452533394 ) ) ;
#17533 = VERTEX_POINT ( 'NONE', #9149 ) ;
#17534 = CARTESIAN_POINT ( 'NONE',  ( 43.01140435219951286, 114.5344580088725479, 39.46799094044489209 ) ) ;
#17535 = LINE ( 'NONE', #20970, #4101 ) ;
#17536 = CARTESIAN_POINT ( 'NONE',  ( 46.59305225739526435, 76.57977050742731251, 36.81289934271958941 ) ) ;
#17537 = CARTESIAN_POINT ( 'NONE',  ( 47.43856463449117200, 136.4651871740939839, 35.64915139335016647 ) ) ;
#17538 = CARTESIAN_POINT ( 'NONE',  ( 48.01140435219951996, 98.21049967264875136, 34.21067981925357060 ) ) ;
#17539 = CARTESIAN_POINT ( 'NONE',  ( 46.60148787037231699, 85.86292235506145687, 7.220022382731924537 ) ) ;
#17540 = EDGE_CURVE ( 'NONE', #20108, #12027, #12221, .T. ) ;
#17541 = CARTESIAN_POINT ( 'NONE',  ( 46.10157429594899270, 119.6604996726487258, 29.95742577749336988 ) ) ;
#17542 = CARTESIAN_POINT ( 'NONE',  ( -157.6495955161842062, -161.0391397928654840, 58.16351966513671812 ) ) ;
#17543 = CARTESIAN_POINT ( 'NONE',  ( -151.4692556286852607, -158.3130981290892692, 39.65701158161629536 ) ) ;
#17544 = CARTESIAN_POINT ( 'NONE',  ( 43.01140435219951286, 144.5344580088726048, 39.21067981925356349 ) ) ;
#17545 = CARTESIAN_POINT ( 'NONE',  ( 48.01140435219951996, 106.2844580088725763, 34.21067981925357060 ) ) ;
#17546 = ORIENTED_EDGE ( 'NONE', *, *, #8131, .T. ) ;
#17547 = CARTESIAN_POINT ( 'NONE',  ( 46.59305225739526435, 85.57977050742732672, 36.81289934271958941 ) ) ;
#17548 = CARTESIAN_POINT ( 'NONE',  ( -159.0959885057557983, -160.5938272943107279, 55.19815736654470584 ) ) ;
#17549 = EDGE_CURVE ( 'NONE', #15960, #17077, #2297, .T. ) ;
#17550 = CARTESIAN_POINT ( 'NONE',  ( 76.20123706073158587, 111.5182621349952257, -8.137091297256032973 ) ) ;
#17551 = CARTESIAN_POINT ( 'NONE',  ( -143.8425227516148084, -192.9584106276440423, 55.19815736654470584 ) ) ;
#17552 = ORIENTED_EDGE ( 'NONE', *, *, #19445, .F. ) ;
#17553 = CARTESIAN_POINT ( 'NONE',  ( 43.01140435219957681, 68.03445800887257633, 29.21067981925356705 ) ) ;
#17554 = VECTOR ( 'NONE', #1284, 1000.000000000000000 ) ;
#17555 = FACE_OUTER_BOUND ( 'NONE', #3040, .T. ) ;
#17556 =( BOUNDED_CURVE ( )  B_SPLINE_CURVE ( 1, ( #15397, #3188 ),
 .UNSPECIFIED., .F., .F. ) 
 B_SPLINE_CURVE_WITH_KNOTS ( ( 2, 2 ),
 ( 0.000000000000000000, 1.000000000000000000 ),
 .UNSPECIFIED. ) 
 CURVE ( )  GEOMETRIC_REPRESENTATION_ITEM ( )  RATIONAL_B_SPLINE_CURVE ( ( 0.9782074146920101132, 0.9782074146920101132 ) ) 
 REPRESENTATION_ITEM ( '' )  );
#17557 = CARTESIAN_POINT ( 'NONE',  ( 46.59305225739526435, 133.5797705074272983, 36.81289934271958941 ) ) ;
#17558 = CARTESIAN_POINT ( 'NONE',  ( 73.43285993012185031, 135.4320224564883688, -7.942088354107054826 ) ) ;
#17559 = EDGE_CURVE ( 'NONE', #1608, #8611, #17609, .T. ) ;
#17560 = ORIENTED_EDGE ( 'NONE', *, *, #20616, .T. ) ;
#17561 = SURFACE_STYLE_USAGE ( .BOTH. , #8884 ) ;
#17562 = ORIENTED_EDGE ( 'NONE', *, *, #11962, .F. ) ;
#17563 = CARTESIAN_POINT ( 'NONE',  ( 46.59305225739526435, 125.1797705074273210, 31.60846029578754468 ) ) ;
#17564 = CARTESIAN_POINT ( 'NONE',  ( 43.01140435219950575, 140.0344580088726332, 29.21067981925357060 ) ) ;
#17565 = CARTESIAN_POINT ( 'NONE',  ( 44.55648932407425633, 155.8104996726487741, 29.45539723777780239 ) ) ;
#17566 = EDGE_CURVE ( 'NONE', #3649, #17523, #5695, .T. ) ;
#17567 = VECTOR ( 'NONE', #11067, 1000.000000000000000 ) ;
#17568 = CARTESIAN_POINT ( 'NONE',  ( 42.21948215057684450, 100.3836182503284533, 39.21067981925355639 ) ) ;
#17569 = CARTESIAN_POINT ( 'NONE',  ( 42.21948215057684450, 130.3836182503284533, 39.21067981925355639 ) ) ;
#17570 = CARTESIAN_POINT ( 'NONE',  ( 45.74753988029933538, 100.1651871740939868, 37.97664729208901946 ) ) ;
#17571 = CARTESIAN_POINT ( 'NONE',  ( 48.01140435219951996, 133.4344580088725820, 32.58608133808903773 ) ) ;
#17572 = DIRECTION ( 'NONE',  ( 0.000000000000000000, 0.000000000000000000, 1.000000000000000000 ) ) ;
#17573 = CARTESIAN_POINT ( 'NONE',  ( -142.0420953463936087, -195.3938272943107393, 49.65701158161630957 ) ) ;
#17574 = CARTESIAN_POINT ( 'NONE',  ( 116.4417310231185780, -126.9891397928655010, 49.65701158161629536 ) ) ;
#17575 = EDGE_CURVE ( 'NONE', #8316, #19257, #1481, .T. ) ;
#17576 = CARTESIAN_POINT ( 'NONE',  ( 48.01140435219951996, 136.2844580088726048, 34.21067981925357060 ) ) ;
#17577 = CARTESIAN_POINT ( 'NONE',  ( 43.01140435219951286, 110.6297705074273097, 29.55568802177586463 ) ) ;
#17578 = CARTESIAN_POINT ( 'NONE',  ( 58.08784223975295902, 95.98046199469133910, 5.794885020722011504 ) ) ;
#17579 = FACE_OUTER_BOUND ( 'NONE', #9306, .T. ) ;
#17580 = CARTESIAN_POINT ( 'NONE',  ( 44.37947211624943833, 101.2151871740939981, 30.00020018409699318 ) ) ;
#17581 = CARTESIAN_POINT ( 'NONE',  ( 116.9721770337685740, 133.1239846058259388, -35.00000000000000000 ) ) ;
#17582 = ORIENTED_EDGE ( 'NONE', *, *, #15449, .F. ) ;
#17583 = CARTESIAN_POINT ( 'NONE',  ( 46.10157429594899270, 76.73445800887256496, 29.95742577749336988 ) ) ;
#17584 = CARTESIAN_POINT ( 'NONE',  ( 71.53613896966024299, 138.8348963267899592, -2.065403804986401859 ) ) ;
#17585 = CARTESIAN_POINT ( 'NONE',  ( 67.71458430423905384, 106.3058120325361671, 6.227933542621733487 ) ) ;
#17586 = DIRECTION ( 'NONE',  ( 0.000000000000000000, 0.000000000000000000, 1.000000000000000000 ) ) ;
#17587 = AXIS2_PLACEMENT_3D ( 'NONE', #11419, #6590, #4932 ) ;
#17588 = CARTESIAN_POINT ( 'NONE',  ( 38.58424406990785371, 75.22977050742730398, 32.77220824515697473 ) ) ;
#17589 = ORIENTED_EDGE ( 'NONE', *, *, #12708, .T. ) ;
#17590 = EDGE_CURVE ( 'NONE', #18280, #5724, #4068, .T. ) ;
#17591 = VERTEX_POINT ( 'NONE', #8824 ) ;
#17592 = CARTESIAN_POINT ( 'NONE',  ( 46.59305225739526435, 151.5797705074273267, 36.81289934271958941 ) ) ;
#17593 = CARTESIAN_POINT ( 'NONE',  ( -148.3790856849358306, -165.6630981290892919, 59.16757674456786020 ) ) ;
#17594 = CARTESIAN_POINT ( 'NONE',  ( 41.46631938032478359, 121.3104996726487457, 38.96596240072933170 ) ) ;
#17596 = CARTESIAN_POINT ( 'NONE',  ( 69.90255027150604406, 140.9627200460241454, -1.156626220813373518 ) ) ;
#17595 = CARTESIAN_POINT ( 'NONE',  ( 46.59305225739526435, 76.91518717409400097, 31.60846029578754468 ) ) ;
#17597 = CARTESIAN_POINT ( 'NONE',  ( -154.3824083646099439, -175.2938272943107165, 58.62277379824867296 ) ) ;
#17598 = CARTESIAN_POINT ( 'NONE',  ( 12.61881386508366809, 104.1535352963828984, 15.55354899318430739 ) ) ;
#17599 = CARTESIAN_POINT ( 'NONE',  ( -159.5594255724347761, -187.8630981290893089, 43.77915905869157598 ) ) ;
#17600 = COLOUR_RGB ( '', 0.31764706, 0.68627451, 0.89019608) ;
#17601 = CARTESIAN_POINT ( 'NONE',  ( 18.01140435219953062, 119.9070776186055838, 50.00000000000002842 ) ) ;
#17602 = CARTESIAN_POINT ( 'NONE',  ( 46.10157429594899270, 157.7344580088726218, 29.95742577749337343 ) ) ;
#17603 = CARTESIAN_POINT ( 'NONE',  ( 39.42975644700377558, 141.0797705074273267, 31.60846029578754468 ) ) ;
#17604 = CARTESIAN_POINT ( 'NONE',  ( 77.28446211531542076, 118.2294073780637262, 4.644197663618684579 ) ) ;
#17605 = CARTESIAN_POINT ( 'NONE',  ( 46.59305225739526435, 124.9151871740940010, 31.60846029578754468 ) ) ;
#17606 = DIRECTION ( 'NONE',  ( -0.4938165983075539223, 0.8695660798558990656, 0.000000000000000000 ) ) ;
#17607 = CARTESIAN_POINT ( 'NONE',  ( -151.4692556286852891, -167.9084106276440309, 39.74470866294723947 ) ) ;
#17608 = DIRECTION ( 'NONE',  ( 1.000000000000000000, 0.000000000000000000, 0.000000000000000000 ) ) ;
#17609 = LINE ( 'NONE', #19167, #15204 ) ;
#17610 = CARTESIAN_POINT ( 'NONE',  ( 34.25380259335813093, 93.01594701623474748, 13.77127495354717190 ) ) ;
#17611 = CARTESIAN_POINT ( 'NONE',  ( 38.96631938032478359, 121.0104996726487343, 37.14960608071593384 ) ) ;
#17612 = CARTESIAN_POINT ( 'NONE',  ( 46.59305225739526435, 109.9151871740940010, 31.60846029578754468 ) ) ;
#17613 = ORIENTED_EDGE ( 'NONE', *, *, #9214, .T. ) ;
#17614 = COLOUR_RGB ( '', 0.40784314, 0.44705882, 0.49803922) ;
#17615 = DIRECTION ( 'NONE',  ( 0.000000000000000000, 0.000000000000000000, -1.000000000000000000 ) ) ;
#17616 = ORIENTED_EDGE ( 'NONE', *, *, #7862, .F. ) ;
#17617 = CARTESIAN_POINT ( 'NONE',  ( 38.01140435219951996, 92.93445800887258201, 35.83527830041810347 ) ) ;
#17618 = ADVANCED_FACE ( 'NONE', ( #5716, #653 ), #7390, .F. ) ;
#17619 = CARTESIAN_POINT ( 'NONE',  ( 43.01140435219951286, 149.6297705074273097, 29.55568802177586107 ) ) ;
#17620 = CARTESIAN_POINT ( 'NONE',  ( 47.05648932407426344, 146.5104996726487627, 31.27175355779120025 ) ) ;
#17622 = CARTESIAN_POINT ( 'NONE',  ( 41.47717036631702570, 147.9855288695934803, -2.148757419388624523 ) ) ;
#17621 = CARTESIAN_POINT ( 'NONE',  ( 41.64333658814960870, 108.7151871740940123, 38.42115945441014446 ) ) ;
#17623 =( BOUNDED_CURVE ( )  B_SPLINE_CURVE ( 2, ( #14770, #1330, #21729, #13233, #21513, #16642, #19628, #2764, #1221, #21400, #8283, #6287, #4521 ),
 .UNSPECIFIED., .F., .F. ) 
 B_SPLINE_CURVE_WITH_KNOTS ( ( 3, 2, 2, 2, 2, 2, 3 ),
 ( 0.4485294117647058987, 0.4500000000000000111, 0.4529411764705882359, 0.4558823529411764608, 0.4588235294117646856, 0.4617647058823529660, 0.4632352941176470784 ),
 .UNSPECIFIED. ) 
 CURVE ( )  GEOMETRIC_REPRESENTATION_ITEM ( )  RATIONAL_B_SPLINE_CURVE ( ( 0.9755282581475768211, 0.9755282581475768211, 1.000000000000000000, 0.9510565162951535312, 1.000000000000000000, 0.9510565162951535312, 1.000000000000000000, 0.9510565162951535312, 1.000000000000000000, 0.9510565162951535312, 1.000000000000000000, 0.9755282581475768211, 0.9755282581475768211 ) ) 
 REPRESENTATION_ITEM ( '' )  );
#17624 = CARTESIAN_POINT ( 'NONE',  ( 38.01140435219951996, 63.86049967264874283, 35.83527830041810347 ) ) ;
#17626 = CARTESIAN_POINT ( 'NONE',  ( -153.0531000319306827, -158.2362167067690280, 39.65701158161629536 ) ) ;
#17625 = CARTESIAN_POINT ( 'NONE',  ( -151.4692556286852607, -167.3130981290893260, 39.65701158161629536 ) ) ;
#17627 = CARTESIAN_POINT ( 'NONE',  ( 111.4021762516569964, 137.5714195593754710, 4.000000000000003553 ) ) ;
#17628 = CARTESIAN_POINT ( 'NONE',  ( -94.10404323627655288, -13.18023274290474767, -19.99999999999997868 ) ) ;
#17629 = CARTESIAN_POINT ( 'NONE',  ( 45.74753988029933538, 73.16518717409400097, 37.97664729208901946 ) ) ;
#17630 = CARTESIAN_POINT ( 'NONE',  ( 26.28921445626723852, 149.7786157371718616, -3.732453678475698311 ) ) ;
#17631 = CARTESIAN_POINT ( 'NONE',  ( -142.0420953463935803, -171.5438272943106881, 52.72008163687743831 ) ) ;
#17632 = CARTESIAN_POINT ( 'NONE',  ( -148.5561028927606344, -193.2584106276440252, 58.62277379824867296 ) ) ;
#17633 = ORIENTED_EDGE ( 'NONE', *, *, #13309, .F. ) ;
#17634 = CARTESIAN_POINT ( 'NONE',  ( -160.8964159109769696, -179.0084106276440252, 52.72008163687743121 ) ) ;
#17635 = CARTESIAN_POINT ( 'NONE',  ( 11.58389279593228238, 133.6817500236834917, 1.549157854527217104 ) ) ;
#17636 = ADVANCED_FACE ( 'NONE', ( #15533 ), #15634, .T. ) ;
#17637 = ORIENTED_EDGE ( 'NONE', *, *, #17954, .F. ) ;
#17638 = CARTESIAN_POINT ( 'NONE',  ( 38.58424406990786082, 135.1151871740940180, 34.21067981925357060 ) ) ;
#17639 = CARTESIAN_POINT ( 'NONE',  ( 39.42975644700377558, 99.07977050742732672, 31.60846029578754468 ) ) ;
#17640 = ORIENTED_EDGE ( 'NONE', *, *, #3591, .F. ) ;
#17641 = ORIENTED_EDGE ( 'NONE', *, *, #14159, .T. ) ;
#17642 = VECTOR ( 'NONE', #9532, 1000.000000000000000 ) ;
#17643 = CARTESIAN_POINT ( 'NONE',  ( 47.24326884731692644, 147.7868190896643341, 4.084992211255583427 ) ) ;
#17644 = VERTEX_POINT ( 'NONE', #13872 ) ;
#17645 = CARTESIAN_POINT ( 'NONE',  ( 47.05648932407426344, 112.5844580088725877, 31.27175355779120025 ) ) ;
#17646 = CARTESIAN_POINT ( 'NONE',  ( -176.9699209214867324, -126.9891397928655010, -72.64809332337415526 ) ) ;
#17647 = CARTESIAN_POINT ( 'NONE',  ( 46.59305225739526435, 77.17977050742732104, 31.60846029578754468 ) ) ;
#17648 = CARTESIAN_POINT ( 'NONE',  ( 39.42975644700377558, 132.4151871740940010, 36.81289934271958941 ) ) ;
#17649 = CARTESIAN_POINT ( 'NONE',  ( 38.96631938032478359, 94.01049967264873430, 37.14960608071593384 ) ) ;
#17650 = CARTESIAN_POINT ( 'NONE',  ( 10.16827731527805767, 110.2528774685086574, 8.767718578943870966 ) ) ;
#17651 = CARTESIAN_POINT ( 'NONE',  ( 42.68471116819608113, 94.90707761860558378, 29.21067981925357415 ) ) ;
#17652 = EDGE_CURVE ( 'NONE', #7609, #6509, #13062, .T. ) ;
#17653 = CARTESIAN_POINT ( 'NONE',  ( -161.4692556286852607, -158.3391397928654385, 52.90620854394536821 ) ) ;
#17654 = CARTESIAN_POINT ( 'NONE',  ( -145.2889157411863437, -159.5130981290892862, 58.16351966513671812 ) ) ;
#17655 = CARTESIAN_POINT ( 'NONE',  ( 46.10157429594899270, 63.83445800887258059, 38.46393386101375711 ) ) ;
#17656 = CARTESIAN_POINT ( 'NONE',  ( 43.01140435219951286, 143.0344580088726048, 29.21067981925356705 ) ) ;
#17657 = AXIS2_PLACEMENT_3D ( 'NONE', #7441, #15902, #19225 ) ;
#17658 = VERTEX_POINT ( 'NONE', #20610 ) ;
#17659 = CARTESIAN_POINT ( 'NONE',  ( 47.43856463449117200, 77.02977050742731535, 32.77220824515698183 ) ) ;
#17660 = CARTESIAN_POINT ( 'NONE',  ( -145.6429501568359797, -161.9438272943107222, 41.63779006702063867 ) ) ;
#17661 = CARTESIAN_POINT ( 'NONE',  ( 47.47886434171987702, 153.8471147930492862, -3.017879606865911502 ) ) ;
#17662 = CARTESIAN_POINT ( 'NONE',  ( -148.5561028927606344, -193.2584106276440252, 58.62277379824867296 ) ) ;
#17663 = AXIS2_PLACEMENT_3D ( 'NONE', #15605, #1847, #17040 ) ;
#17664 = ORIENTED_EDGE ( 'NONE', *, *, #12750, .T. ) ;
#17665 = CARTESIAN_POINT ( 'NONE',  ( 41.46631938032478359, 68.18445800887256780, 29.45539723777780239 ) ) ;
#17666 = DIRECTION ( 'NONE',  ( 0.000000000000000000, -1.000000000000000000, 0.000000000000000000 ) ) ;
#17667 = CARTESIAN_POINT ( 'NONE',  ( 40.27526882409969744, 135.8297705074273267, 37.97664729208901235 ) ) ;
#17668 = ORIENTED_EDGE ( 'NONE', *, *, #6100, .T. ) ;
#17669 = EDGE_CURVE ( 'NONE', #12279, #1240, #10648, .T. ) ;
#17670 = CARTESIAN_POINT ( 'NONE',  ( -120.0322075325610740, -126.9891397928655010, 49.65701158161630957 ) ) ;
#17671 = ORIENTED_EDGE ( 'NONE', *, *, #10183, .F. ) ;
#17672 = CARTESIAN_POINT ( 'NONE',  ( 39.42975644700377558, 123.0797705074273267, 31.60846029578754468 ) ) ;
#17673 = CARTESIAN_POINT ( 'NONE',  ( 44.55648932407425633, 138.6844580088725820, 38.96596240072933170 ) ) ;
#17674 = EDGE_CURVE ( 'NONE', #12379, #14777, #439, .T. ) ;
#17675 = B_SPLINE_CURVE_WITH_KNOTS ( 'NONE', 3,
 ( #4835, #5563, #3921, #7452, #17354, #13940, #19131, #10755 ),
 .UNSPECIFIED., .F., .F.,
 ( 4, 2, 2, 4 ),
 ( 0.002864483144845920981, 0.004294853615569181084, 0.005010038850930821110, 0.005725224086292461136 ),
 .UNSPECIFIED. ) ;
#17676 = CARTESIAN_POINT ( 'NONE',  ( 41.46631938032478359, 110.1844580088725820, 29.45539723777780239 ) ) ;
#17677 = CARTESIAN_POINT ( 'NONE',  ( 41.46631938032478359, 130.3104996726487457, 38.96596240072933170 ) ) ;
#17678 = CARTESIAN_POINT ( 'NONE',  ( -161.4692556286852607, -191.6391397928654214, 46.40781461928724383 ) ) ;
#17679 = CARTESIAN_POINT ( 'NONE',  ( 43.01140435219951286, 90.53445800887257633, 39.21067981925356349 ) ) ;
#17680 = CARTESIAN_POINT ( 'NONE',  ( -151.4692556286852607, -159.8130981290892692, 59.65701158161632378 ) ) ;
#17681 = CARTESIAN_POINT ( 'NONE',  ( -141.4692556286852891, -162.2130981290893033, 52.90620854394536821 ) ) ;
#17682 = APPLICATION_PROTOCOL_DEFINITION ( 'draft international standard', 'automotive_design', 1998, #11668 ) ;
#17683 = CARTESIAN_POINT ( 'NONE',  ( 46.10157429594899270, 130.7344580088725934, 29.95742577749337343 ) ) ;
#17684 = CARTESIAN_POINT ( 'NONE',  ( 44.37947211624943833, 112.2797705074273296, 38.42115945441014446 ) ) ;
#17685 =( BOUNDED_CURVE ( )  B_SPLINE_CURVE ( 2, ( #2772, #7960, #9513, #16212, #21299 ),
 .UNSPECIFIED., .F., .F. ) 
 B_SPLINE_CURVE_WITH_KNOTS ( ( 3, 2, 3 ),
 ( 0.9779411764705882026, 0.9794117647058823151, 0.9803958342062289999 ),
 .UNSPECIFIED. ) 
 CURVE ( )  GEOMETRIC_REPRESENTATION_ITEM ( )  RATIONAL_B_SPLINE_CURVE ( ( 0.9755282581475768211, 0.9755282581475768211, 1.000000000000000000, 0.9836243115514174962, 0.9782066976764471899 ) ) 
 REPRESENTATION_ITEM ( '' )  );
#17686 = CARTESIAN_POINT ( 'NONE',  ( 55.13406075593908895, 145.4575617026882526, 3.413969760132236964 ) ) ;
#17687 = CARTESIAN_POINT ( 'NONE',  ( -143.8425227516148084, -192.0938272943107279, 44.11586579668791330 ) ) ;
#17688 = CARTESIAN_POINT ( 'NONE',  ( 39.42975644700377558, 93.41518717409400097, 36.81289934271958941 ) ) ;
#17689 = DIRECTION ( 'NONE',  ( -0.000000000000000000, -0.000000000000000000, -1.000000000000000000 ) ) ;
#17690 = ORIENTED_EDGE ( 'NONE', *, *, #315, .T. ) ;
#17691 = CARTESIAN_POINT ( 'NONE',  ( 38.96631938032478359, 87.41049967264873999, 31.27175355779120025 ) ) ;
#17692 = CARTESIAN_POINT ( 'NONE',  ( 66.89036333300305159, 144.4373801540182569, -2.303882249869787291 ) ) ;
#17693 = CARTESIAN_POINT ( 'NONE',  ( 71.06985403747866314, 121.7623127629220932, -14.41049859375789666 ) ) ;
#17694 = CARTESIAN_POINT ( 'NONE',  ( 8.944919112598912037, 123.2842988173194385, -4.803623532975393573 ) ) ;
#17695 = CARTESIAN_POINT ( 'NONE',  ( 43.01140435219951286, 79.12977050742732388, 38.86567161673127657 ) ) ;
#17696 = ORIENTED_EDGE ( 'NONE', *, *, #20278, .F. ) ;
#17697 = ORIENTED_EDGE ( 'NONE', *, *, #12686, .F. ) ;
#17698 = CARTESIAN_POINT ( 'NONE',  ( 46.59305225739526435, 158.1797705074273210, 31.60846029578754468 ) ) ;
#17699 = DIRECTION ( 'NONE',  ( 1.000000000000000000, 0.000000000000000000, 0.000000000000000000 ) ) ;
#17700 = CARTESIAN_POINT ( 'NONE',  ( 46.10157429594899270, 119.6604996726487400, 29.95742577749337343 ) ) ;
#17702 = CARTESIAN_POINT ( 'NONE',  ( 8.987667018801221985, 116.9306527918008527, -4.013769077970609445 ) ) ;
#17701 = CARTESIAN_POINT ( 'NONE',  ( 41.64333658814960870, 78.71518717409399812, 38.42115945441014446 ) ) ;
#17703 = CARTESIAN_POINT ( 'NONE',  ( -151.4692556286852891, -167.6438272943106824, 39.74470866294723947 ) ) ;
#17704 = CARTESIAN_POINT ( 'NONE',  ( 21.90415124324598750, 92.95514585177724598, 15.07745334355238676 ) ) ;
#17705 = CARTESIAN_POINT ( 'NONE',  ( -157.6495955161842062, -190.1130981290892805, 58.16351966513671812 ) ) ;
#17706 =( NAMED_UNIT ( * ) SI_UNIT ( $, .STERADIAN. ) SOLID_ANGLE_UNIT ( ) );
#17707 = CARTESIAN_POINT ( 'NONE',  ( 161.4773229304660731, 84.89323405393692212, 4.000000000000021316 ) ) ;
#17708 = CARTESIAN_POINT ( 'NONE',  ( 43.01140435219951996, 150.5344580088725763, 39.21067981925356349 ) ) ;
#17709 = CARTESIAN_POINT ( 'NONE',  ( 76.90526227772885193, 114.5556580205831096, 4.763324653225488703 ) ) ;
#17710 = CARTESIAN_POINT ( 'NONE',  ( 38.58424406990786082, 129.1151871740940180, 34.21067981925357060 ) ) ;
#17711 = CARTESIAN_POINT ( 'NONE',  ( 41.46631938032478359, 69.11049967264872862, 29.45539723777780239 ) ) ;
#17712 = CARTESIAN_POINT ( 'NONE',  ( -142.0420953463935803, -159.8084106276440650, 52.72008163687743831 ) ) ;
#17713 = CARTESIAN_POINT ( 'NONE',  ( -151.4692556286853176, -165.2391397928654442, 39.65701158161629536 ) ) ;
#17714 = CARTESIAN_POINT ( 'NONE',  ( 131.8222645499855901, 267.5435007770738025, -6.999999999999995559 ) ) ;
#17715 = CARTESIAN_POINT ( 'NONE',  ( 16.54882264740998110, 129.8072851447780067, 22.56993813403257931 ) ) ;
#17716 = CARTESIAN_POINT ( 'NONE',  ( 40.27526882409969033, 107.6651871740940152, 30.44471234641811819 ) ) ;
#17717 = EDGE_CURVE ( 'NONE', #11079, #8083, #129, .T. ) ;
#17718 = ORIENTED_EDGE ( 'NONE', *, *, #1662, .F. ) ;
#17719 = CARTESIAN_POINT ( 'NONE',  ( 43.01140435219951996, 119.9070776186055838, -35.00000000000000000 ) ) ;
#17720 = VERTEX_POINT ( 'NONE', #2619 ) ;
#17721 = CARTESIAN_POINT ( 'NONE',  ( 48.01140435219951996, 88.43445800887258201, 32.58608133808903773 ) ) ;
#17722 = CARTESIAN_POINT ( 'NONE',  ( 89.42064422693164261, 282.0082918409407284, 4.000000000000003553 ) ) ;
#17723 = AXIS2_PLACEMENT_3D ( 'NONE', #12522, #16147, #17901 ) ;
#17724 = CARTESIAN_POINT ( 'NONE',  ( 46.10157429594899270, 149.6604996726486831, 29.95742577749337343 ) ) ;
#17726 = CARTESIAN_POINT ( 'NONE',  ( 49.32098446784893753, 92.50438258598539676, -5.839070001793449372 ) ) ;
#17725 = CARTESIAN_POINT ( 'NONE',  ( 38.58424406990784661, 102.2651871740939811, 35.64915139335016647 ) ) ;
#17727 = CARTESIAN_POINT ( 'NONE',  ( 38.01140435219951996, 66.86049967264874283, 35.83527830041810347 ) ) ;
#17729 = CARTESIAN_POINT ( 'NONE',  ( 44.55648932407425633, 60.68445800887258201, 38.96596240072933170 ) ) ;
#17728 = CARTESIAN_POINT ( 'NONE',  ( 147.5268905834513475, 193.0332408774651185, -29.99999999999997868 ) ) ;
#17730 = CARTESIAN_POINT ( 'NONE',  ( -161.4692556286853176, -187.5630981290892976, 49.65701158161630957 ) ) ;
#17731 = FACE_OUTER_BOUND ( 'NONE', #7085, .T. ) ;
#17732 = CARTESIAN_POINT ( 'NONE',  ( 46.59305225739526435, 73.31518717409400665, 36.81289934271958941 ) ) ;
#17733 = CARTESIAN_POINT ( 'NONE',  ( -151.4692556286852891, -126.9891397928655010, 49.65701158161630957 ) ) ;
#17734 = AXIS2_PLACEMENT_3D ( 'NONE', #1888, #19868, #13139 ) ;
#17735 = DIRECTION ( 'NONE',  ( -0.000000000000000000, -0.000000000000000000, 1.000000000000000000 ) ) ;
#17736 = CARTESIAN_POINT ( 'NONE',  ( -157.2955611005346270, -167.3438272943106995, 41.63779006702063867 ) ) ;
#17737 = CARTESIAN_POINT ( 'NONE',  ( -142.0420953463936087, -183.6584106276440309, 49.65701158161630957 ) ) ;
#17738 = EDGE_LOOP ( 'NONE', ( #13821, #142, #8935, #8200 ) ) ;
#17739 = VECTOR ( 'NONE', #18509, 1000.000000000000000 ) ;
#17740 = CARTESIAN_POINT ( 'NONE',  ( -160.8964159109769696, -173.3084106276440366, 46.59394152635518793 ) ) ;
#17741 = CARTESIAN_POINT ( 'NONE',  ( 26.06094713673110164, 149.7432261477326563, 2.263147435255992601 ) ) ;
#17742 = ORIENTED_EDGE ( 'NONE', *, *, #20930, .F. ) ;
#17743 = CARTESIAN_POINT ( 'NONE',  ( 40.27526882409969033, 135.5651871740939782, 37.97664729208901946 ) ) ;
#17744 = EDGE_CURVE ( 'NONE', #20615, #1337, #19709, .T. ) ;
#17745 = CARTESIAN_POINT ( 'NONE',  ( 47.43856463449117911, 154.4651871740940123, 35.64915139335015937 ) ) ;
#17746 = CARTESIAN_POINT ( 'NONE',  ( 38.58424406990786082, 93.37977050742732388, 34.21067981925357060 ) ) ;
#17747 = ORIENTED_EDGE ( 'NONE', *, *, #13847, .T. ) ;
#17748 = VERTEX_POINT ( 'NONE', #1300 ) ;
#17749 = CARTESIAN_POINT ( 'NONE',  ( 35.91077447413180579, 147.1981228300969633, 10.63281669705329691 ) ) ;
#17750 = ORIENTED_EDGE ( 'NONE', *, *, #3313, .T. ) ;
#17751 = CARTESIAN_POINT ( 'NONE',  ( 48.01140435219951996, 118.4344580088725820, 32.58608133808903773 ) ) ;
#17752 = CIRCLE ( 'NONE', #19523, 2.999999999999997780 ) ;
#17753 = LINE ( 'NONE', #9834, #5493 ) ;
#17754 = CARTESIAN_POINT ( 'NONE',  ( 41.64333658814960870, 78.97977050742731819, 38.42115945441014446 ) ) ;
#17755 = CARTESIAN_POINT ( 'NONE',  ( 40.27526882409969033, 134.6651871740940294, 30.44471234641811819 ) ) ;
#17756 = CARTESIAN_POINT ( 'NONE',  ( 44.55648932407425633, 89.81049967264874567, 29.45539723777780239 ) ) ;
#17757 = CARTESIAN_POINT ( 'NONE',  ( 49.46632042442519861, 86.28835692931116341, 14.12497754236212977 ) ) ;
#17758 = CARTESIAN_POINT ( 'NONE',  ( 38.94332714213889091, 95.24011124016369934, 37.12229684998503387 ) ) ;
#17759 = CARTESIAN_POINT ( 'NONE',  ( -145.2889157411863721, -162.5391397928654271, 41.15050349809590102 ) ) ;
#17760 = CARTESIAN_POINT ( 'NONE',  ( -148.3790856849358306, -158.4630981290893317, 40.14644641866477315 ) ) ;
#17761 = CARTESIAN_POINT ( 'NONE',  ( 134.3985507411545939, 186.9327686461008682, 21.73429951086134082 ) ) ;
#17762 = CYLINDRICAL_SURFACE ( 'NONE', #1480, 24.99999999999998579 ) ;
#17763 = ORIENTED_EDGE ( 'NONE', *, *, #11114, .F. ) ;
#17764 = CARTESIAN_POINT ( 'NONE',  ( 41.64333658814960870, 72.97977050742731819, 38.42115945441014446 ) ) ;
#17765 = CARTESIAN_POINT ( 'NONE',  ( -151.4692556286852891, -163.1438272943106824, 59.56931450028537967 ) ) ;
#17766 = CARTESIAN_POINT ( 'NONE',  ( 43.80529445460960858, 154.1304981347762748, -3.137004163733609907 ) ) ;
#17767 = CARTESIAN_POINT ( 'NONE',  ( -156.3976848494337162, -155.9071947501682018, 41.12080071780688684 ) ) ;
#17768 = ORIENTED_EDGE ( 'NONE', *, *, #18588, .T. ) ;
#17769 = LINE ( 'NONE', #11488, #13600 ) ;
#17770 = CARTESIAN_POINT ( 'NONE',  ( 43.80332655382220253, 124.9575765865522925, 29.21067981925356705 ) ) ;
#17771 = CARTESIAN_POINT ( 'NONE',  ( 38.58424406990786082, 120.3797705074273239, 34.21067981925357060 ) ) ;
#17772 = ORIENTED_EDGE ( 'NONE', *, *, #15749, .T. ) ;
#17773 = VECTOR ( 'NONE', #13081, 1000.000000000000000 ) ;
#17774 = CARTESIAN_POINT ( 'NONE',  ( 43.01140435219951286, 89.03445800887257633, 29.21067981925356705 ) ) ;
#17775 = ORIENTED_EDGE ( 'NONE', *, *, #14009, .T. ) ;
#17776 = CARTESIAN_POINT ( 'NONE',  ( 45.74753988029933538, 127.4297705074273068, 37.97664729208901946 ) ) ;
#17777 = CARTESIAN_POINT ( 'NONE',  ( 18.01140435219953062, 119.9070776186055838, -19.99999999999997868 ) ) ;
#17778 = CARTESIAN_POINT ( 'NONE',  ( 38.01140435219952707, 59.78445800887258343, 34.21067981925357060 ) ) ;
#17779 = CARTESIAN_POINT ( 'NONE',  ( 38.01140435219952707, 110.7844580088725905, 34.21067981925357060 ) ) ;
#17780 = CARTESIAN_POINT ( 'NONE',  ( 43.01140435219951286, 83.03445800887257633, 29.21067981925356705 ) ) ;
#17781 = DIRECTION ( 'NONE',  ( 0.000000000000000000, 0.000000000000000000, 1.000000000000000000 ) ) ;
#17782 = CARTESIAN_POINT ( 'NONE',  ( -148.3790856849358306, -186.3891397928654783, 40.14644641866477315 ) ) ;
#17783 = ADVANCED_FACE ( 'NONE', ( #4600 ), #13094, .F. ) ;
#17784 = CARTESIAN_POINT ( 'NONE',  ( 39.92123440845005433, 67.16049967264873999, 38.46393386101375711 ) ) ;
#17785 = CARTESIAN_POINT ( 'NONE',  ( 136.2461330483349968, 181.9161108113851526, 22.68744729171066155 ) ) ;
#17786 = CARTESIAN_POINT ( 'NONE',  ( -145.2889157411863721, -158.6130981290893089, 41.15050349809590102 ) ) ;
#17787 = APPLICATION_PROTOCOL_DEFINITION ( 'draft international standard', 'automotive_design', 1998, #5614 ) ;
#17788 = CARTESIAN_POINT ( 'NONE',  ( 38.01140435219952707, 137.7844580088726048, 34.21067981925357060 ) ) ;
#17789 = CARTESIAN_POINT ( 'NONE',  ( 38.58424406990784661, 105.2297705074273040, 32.77220824515698183 ) ) ;
#17790 = CARTESIAN_POINT ( 'NONE',  ( 67.88957565821384321, 106.4565162521658976, 12.22353771717463466 ) ) ;
#17791 = CARTESIAN_POINT ( 'NONE',  ( -142.0420953463935803, -192.2438272943107336, 46.59394152635518793 ) ) ;
#17792 = CARTESIAN_POINT ( 'NONE',  ( 38.58424406990786082, 102.1151871740940180, 34.21067981925357060 ) ) ;
#17793 = LINE ( 'NONE', #4350, #20700 ) ;
#17794 = VERTEX_POINT ( 'NONE', #973 ) ;
#17795 = CARTESIAN_POINT ( 'NONE',  ( 139.9279279298906147, 262.8829071470229906, -5.999999999999976019 ) ) ;
#17796 = CARTESIAN_POINT ( 'NONE',  ( 71.03835150376274044, 100.2492380157770526, 6.267546321443639989 ) ) ;
#17797 = CARTESIAN_POINT ( 'NONE',  ( 20.50804704269433998, 103.0453634090187762, -11.55335571609641399 ) ) ;
#17798 = CARTESIAN_POINT ( 'NONE',  ( 9.616596702810701558, 112.3753283828585694, -5.161025107254184618 ) ) ;
#17799 = CARTESIAN_POINT ( 'NONE',  ( 45.74753988029934249, 79.42977050742732104, 37.97664729208901235 ) ) ;
#17800 = ORIENTED_EDGE ( 'NONE', *, *, #17075, .F. ) ;
#17801 = VERTEX_POINT ( 'NONE', #1085 ) ;
#17802 = CARTESIAN_POINT ( 'NONE',  ( 47.43856463449118621, 154.8797705074273097, 34.21067981925357060 ) ) ;
#17803 = VECTOR ( 'NONE', #13671, 1000.000000000000114 ) ;
#17804 = FACE_OUTER_BOUND ( 'NONE', #8180, .T. ) ;
#17805 = CARTESIAN_POINT ( 'NONE',  ( 44.55648932407425633, 122.8104996726487457, 29.45539723777780239 ) ) ;
#17807 = CARTESIAN_POINT ( 'NONE',  ( 56.91482361236938203, 88.71218622616480332, 0.8673887411229855848 ) ) ;
#17806 = CARTESIAN_POINT ( 'NONE',  ( 45.74753988029933538, 79.16518717409398675, 37.97664729208901946 ) ) ;
#17808 = DIRECTION ( 'NONE',  ( 1.000000000000000000, 0.000000000000000000, 0.000000000000000000 ) ) ;
#17809 =( BOUNDED_CURVE ( )  B_SPLINE_CURVE ( 2, ( #12051, #20335, #158, #3794, #5539, #11839, #5433, #1916, #3685, #13496, #15576, #8651, #10523 ),
 .UNSPECIFIED., .F., .F. ) 
 B_SPLINE_CURVE_WITH_KNOTS ( ( 3, 2, 2, 2, 2, 2, 3 ),
 ( 0.3035714285714286031, 0.3071428571428571619, 0.3142857142857142794, 0.3214285714285714524, 0.3285714285714285698, 0.3357142857142856873, 0.3392857142857142461 ),
 .UNSPECIFIED. ) 
 CURVE ( )  GEOMETRIC_REPRESENTATION_ITEM ( )  RATIONAL_B_SPLINE_CURVE ( ( 0.9755282581475768211, 0.9755282581475769321, 1.000000000000000000, 0.9510565162951535312, 1.000000000000000000, 0.9510565162951535312, 1.000000000000000000, 0.9510565162951535312, 1.000000000000000000, 0.9510565162951535312, 1.000000000000000000, 0.9755282581475769321, 0.9755282581475768211 ) ) 
 REPRESENTATION_ITEM ( '' )  );
#17810 = CARTESIAN_POINT ( 'NONE',  ( -148.5561028927606344, -174.9938272943107336, 58.62277379824867296 ) ) ;
#17811 = CARTESIAN_POINT ( 'NONE',  ( 16.30372524420941716, 141.3216567370616019, 9.839263250375132941 ) ) ;
#17812 = CARTESIAN_POINT ( 'NONE',  ( -145.2889157411863721, -192.5130981290892862, 58.16351966513671812 ) ) ;
#17813 = FACE_OUTER_BOUND ( 'NONE', #892, .T. ) ;
#17814 = DIRECTION ( 'NONE',  ( 0.4938165983075534782, -0.8695660798558993987, 0.000000000000000000 ) ) ;
#17815 = CARTESIAN_POINT ( 'NONE',  ( 46.59305225739526435, 133.5797705074272983, 36.81289934271958941 ) ) ;
#17816 = CARTESIAN_POINT ( 'NONE',  ( 63.99609067623438108, 147.0574274800572425, 3.572798616028722396 ) ) ;
#17817 = CIRCLE ( 'NONE', #16776, 10.00000000000000888 ) ;
#17818 = CARTESIAN_POINT ( 'NONE',  ( 39.42975644700377558, 129.4151871740940010, 36.81289934271958941 ) ) ;
#17819 = DIRECTION ( 'NONE',  ( 0.8695660798558991766, 0.4938165983075539778, 0.000000000000000000 ) ) ;
#17820 = CARTESIAN_POINT ( 'NONE',  ( -160.8964159109769696, -158.0084106276439968, 52.72008163687743121 ) ) ;
#17821 = EDGE_CURVE ( 'NONE', #19772, #7040, #6255, .T. ) ;
#17822 = DIRECTION ( 'NONE',  ( 1.000000000000000000, -1.387778780781445676E-16, 0.000000000000000000 ) ) ;
#17823 = AXIS2_PLACEMENT_3D ( 'NONE', #14367, #10537, #7445 ) ;
#17824 = CARTESIAN_POINT ( 'NONE',  ( 41.46631938032478359, 135.1104996726487286, 29.45539723777780239 ) ) ;
#17825 = EDGE_CURVE ( 'NONE', #20615, #2815, #13892, .T. ) ;
#17826 = CARTESIAN_POINT ( 'NONE',  ( 22.30625593121589390, 139.1551866335812235, 23.00981086756132044 ) ) ;
#17827 = CARTESIAN_POINT ( 'NONE',  ( 43.01140435219951996, 10.71049967264875491, 29.21067981925357060 ) ) ;
#17828 = CARTESIAN_POINT ( 'NONE',  ( 46.59305225739526435, 106.3151871740939924, 36.81289934271958941 ) ) ;
#17829 = ORIENTED_EDGE ( 'NONE', *, *, #15076, .F. ) ;
#17830 = CARTESIAN_POINT ( 'NONE',  ( 44.55648932407425633, 86.81049967264874567, 29.45539723777780239 ) ) ;
#17831 = EDGE_LOOP ( 'NONE', ( #14721, #7607, #20643, #21186 ) ) ;
#17832 = CARTESIAN_POINT ( 'NONE',  ( 48.01140435219951996, 91.28445800887257633, 34.21067981925357060 ) ) ;
#17833 = DIRECTION ( 'NONE',  ( 0.000000000000000000, 1.000000000000000000, 0.000000000000000000 ) ) ;
#17834 = CIRCLE ( 'NONE', #19263, 5.000000000000004441 ) ;
#17835 = CARTESIAN_POINT ( 'NONE',  ( 43.01140435219951286, 149.9604996726487514, 28.95336869806222779 ) ) ;
#17837 = CARTESIAN_POINT ( 'NONE',  ( 43.85786119575681852, 148.0137586191354444, -9.053472026759274982 ) ) ;
#17836 = CARTESIAN_POINT ( 'NONE',  ( 38.58424406990784661, 108.2651871740939953, 35.64915139335016647 ) ) ;
#17838 = CARTESIAN_POINT ( 'NONE',  ( 41.46631938032478359, 64.31049967264873146, 38.96596240072933170 ) ) ;
#17840 = CARTESIAN_POINT ( 'NONE',  ( -151.4692556286852607, -158.3130981290892692, 39.65701158161629536 ) ) ;
#17839 = DIRECTION ( 'NONE',  ( -0.3428981916074304581, 0.9393725726208712601, 0.000000000000000000 ) ) ;
#17841 =( NAMED_UNIT ( * ) SI_UNIT ( $, .STERADIAN. ) SOLID_ANGLE_UNIT ( ) );
#17842 = ADVANCED_FACE ( 'NONE', ( #4487 ), #867, .T. ) ;
#17843 = CARTESIAN_POINT ( 'NONE',  ( -161.4692556286852891, -187.7130981290893033, 46.40781461928724383 ) ) ;
#17844 = DIRECTION ( 'NONE',  ( 0.000000000000000000, 0.000000000000000000, -1.000000000000000000 ) ) ;
#17845 = CARTESIAN_POINT ( 'NONE',  ( 40.27526882409969033, 158.9297705074272642, 30.44471234641811819 ) ) ;
#17846 = CARTESIAN_POINT ( 'NONE',  ( 11.74529739132928619, 133.8467647624810581, -4.446451035385589279 ) ) ;
#17847 = CARTESIAN_POINT ( 'NONE',  ( -154.3824083646099439, -170.4938272943107336, 40.69124936498395328 ) ) ;
#17848 = CARTESIAN_POINT ( 'NONE',  ( -143.8425227516148084, -180.9584106276440707, 55.19815736654470584 ) ) ;
#17849 = ORIENTED_EDGE ( 'NONE', *, *, #13509, .F. ) ;
#17850 = CARTESIAN_POINT ( 'NONE',  ( 43.01140435219951286, 66.86518717409397539, 38.86567161673127657 ) ) ;
#17851 = CARTESIAN_POINT ( 'NONE',  ( -160.8964159109769696, -167.0084106276440536, 52.72008163687743121 ) ) ;
#17852 = CARTESIAN_POINT ( 'NONE',  ( 71.22865828484523831, 100.3801644121689094, 12.26314743512348926 ) ) ;
#17853 = AXIS2_PLACEMENT_3D ( 'NONE', #9868, #7998, #12949 ) ;
#17854 = CARTESIAN_POINT ( 'NONE',  ( 44.37947211624943833, 133.0151871740939953, 38.42115945441014446 ) ) ;
#17855 = CARTESIAN_POINT ( 'NONE',  ( 45.74753988029934249, 154.1651871740939725, 37.97664729208901235 ) ) ;
#17856 = VERTEX_POINT ( 'NONE', #16284 ) ;
#17857 = ORIENTED_EDGE ( 'NONE', *, *, #827, .F. ) ;
#17858 = SURFACE_STYLE_FILL_AREA ( #4413 ) ;
#17859 = ORIENTED_EDGE ( 'NONE', *, *, #21582, .F. ) ;
#17860 = CARTESIAN_POINT ( 'NONE',  ( 48.01140435219951996, 118.1344580088725849, 35.83527830041810347 ) ) ;
#17861 = CARTESIAN_POINT ( 'NONE',  ( 47.43856463449117200, 73.72977050742731819, 35.64915139335016647 ) ) ;
#17862 = CARTESIAN_POINT ( 'NONE',  ( 44.37947211624943833, 137.2151871740940123, 30.00020018409699318 ) ) ;
#17863 = CIRCLE ( 'NONE', #928, 7.500000000000007105 ) ;
#17864 = CARTESIAN_POINT ( 'NONE',  ( 43.01140435219951286, 94.46049967264872294, 39.46799094044489209 ) ) ;
#17865 = MECHANICAL_DESIGN_GEOMETRIC_PRESENTATION_REPRESENTATION (  '', ( #6635 ), #9130 ) ;
#17866 = CARTESIAN_POINT ( 'NONE',  ( 42.21854335081802390, 85.68333463812091111, 14.36287948008016890 ) ) ;
#17867 = CARTESIAN_POINT ( 'NONE',  ( 41.39760859918703062, 94.95739275389902900, 29.46707291594048428 ) ) ;
#17868 = CARTESIAN_POINT ( 'NONE',  ( -159.5594255724347761, -164.1891397928654897, 55.53486410454104316 ) ) ;
#17869 = LINE ( 'NONE', #4653, #15042 ) ;
#17870 = LINE ( 'NONE', #6534, #2525 ) ;
#17871 = EDGE_LOOP ( 'NONE', ( #11048, #4919 ) ) ;
#17872 = CARTESIAN_POINT ( 'NONE',  ( 38.58424406990784661, 75.22977050742730398, 32.77220824515698183 ) ) ;
#17873 = CARTESIAN_POINT ( 'NONE',  ( -145.6429501568359797, -159.8438272943107563, 57.67623309621198047 ) ) ;
#17874 = CARTESIAN_POINT ( 'NONE',  ( 8.927628897234525240, 116.7075971571176751, 1.981832035706394546 ) ) ;
#17875 = CARTESIAN_POINT ( 'NONE',  ( -145.6429501568359797, -186.2084106276440707, 41.63779006702063867 ) ) ;
#17876 = ORIENTED_EDGE ( 'NONE', *, *, #17887, .F. ) ;
#17877 = DIRECTION ( 'NONE',  ( 0.000000000000000000, -1.000000000000000000, 0.000000000000000000 ) ) ;
#17878 = LINE ( 'NONE', #9418, #17642 ) ;
#17879 = CARTESIAN_POINT ( 'NONE',  ( 46.59305225739526435, 124.5797705074273267, 36.81289934271958941 ) ) ;
#17880 = ORIENTED_EDGE ( 'NONE', *, *, #12654, .F. ) ;
#17881 = CARTESIAN_POINT ( 'NONE',  ( 47.05648932407426344, 87.98445800887257917, 37.14960608071593384 ) ) ;
#17882 = EDGE_LOOP ( 'NONE', ( #6194, #18799, #8195, #18742 ) ) ;
#17883 = CARTESIAN_POINT ( 'NONE',  ( 41.64333658814960870, 123.9797705074273324, 38.42115945441014446 ) ) ;
#17884 = LINE ( 'NONE', #20543, #12548 ) ;
#17885 = CARTESIAN_POINT ( 'NONE',  ( 44.37947211624943833, 88.27977050742731535, 38.42115945441014446 ) ) ;
#17886 = CARTESIAN_POINT ( 'NONE',  ( 47.05648932407426344, 61.58445800887258059, 31.27175355779120025 ) ) ;
#17887 = EDGE_CURVE ( 'NONE', #5468, #8397, #7126, .T. ) ;
#17888 = FACE_OUTER_BOUND ( 'NONE', #912, .T. ) ;
#17889 = PLANE ( 'NONE',  #8891 ) ;
#17890 = CARTESIAN_POINT ( 'NONE',  ( -154.5594255724347761, -177.0891397928654669, 40.14644641866476604 ) ) ;
#17891 = CARTESIAN_POINT ( 'NONE',  ( -159.5594255724347761, -185.1891397928654612, 55.53486410454104316 ) ) ;
#17892 = CARTESIAN_POINT ( 'NONE',  ( 44.55648932407425633, 73.61049967264874283, 38.96596240072933170 ) ) ;
#17893 = CARTESIAN_POINT ( 'NONE',  ( 38.01140435219952707, 102.5604996726487457, 32.58608133808903773 ) ) ;
#17894 = CARTESIAN_POINT ( 'NONE',  ( -142.0420953463935803, -186.2438272943107620, 46.59394152635518793 ) ) ;
#17895 =( NAMED_UNIT ( * ) SI_UNIT ( $, .STERADIAN. ) SOLID_ANGLE_UNIT ( ) );
#17896 = CARTESIAN_POINT ( 'NONE',  ( 41.46631938032478359, 125.1844580088725678, 29.45539723777780239 ) ) ;
#17897 = CARTESIAN_POINT ( 'NONE',  ( 47.43856463449117200, 107.0297705074273154, 32.77220824515698183 ) ) ;
#17898 = CARTESIAN_POINT ( 'NONE',  ( 33.70380864093198170, 93.20109254516876263, 20.79496611990781929 ) ) ;
#17899 = CARTESIAN_POINT ( 'NONE',  ( -160.8964159109769696, -185.0438272943107165, 46.59394152635518793 ) ) ;
#17900 = CARTESIAN_POINT ( 'NONE',  ( 47.43856463449117911, 97.46518717409399812, 35.64915139335015937 ) ) ;
#17901 = DIRECTION ( 'NONE',  ( -1.000000000000000000, 0.000000000000000000, 0.000000000000000000 ) ) ;
#17902 = ORIENTED_EDGE ( 'NONE', *, *, #16785, .F. ) ;
#17903 = LINE ( 'NONE', #1497, #20003 ) ;
#17904 = CARTESIAN_POINT ( 'NONE',  ( 74.85601106972485752, 107.3429126181175661, -0.9942341299615756745 ) ) ;
#17905 = CARTESIAN_POINT ( 'NONE',  ( 40.27526882409969744, 144.8297705074273267, 37.97664729208901235 ) ) ;
#17906 = CARTESIAN_POINT ( 'NONE',  ( 23.31543935874208273, 139.7533899986231916, -16.95817871342526573 ) ) ;
#17907 = ADVANCED_FACE ( 'NONE', ( #21262 ), #1190, .T. ) ;
#17908 = CARTESIAN_POINT ( 'NONE',  ( 39.42975644700377558, 69.67977050742732104, 36.81289934271958941 ) ) ;
#17909 = ORIENTED_EDGE ( 'NONE', *, *, #4901, .T. ) ;
#17910 = ORIENTED_EDGE ( 'NONE', *, *, #16479, .F. ) ;
#17911 = CARTESIAN_POINT ( 'NONE',  ( 40.27526882409969033, 150.8297705074273267, 37.97664729208901946 ) ) ;
#17912 = DIRECTION ( 'NONE',  ( -0.000000000000000000, 1.000000000000000000, -0.000000000000000000 ) ) ;
#17913 = CARTESIAN_POINT ( 'NONE',  ( 43.01140435219951286, 113.9604996726487371, 28.95336869806222779 ) ) ;
#17915 = CARTESIAN_POINT ( 'NONE',  ( 20.91437931538276374, 145.9617080342048894, -10.94665030085253044 ) ) ;
#17914 = CARTESIAN_POINT ( 'NONE',  ( 45.74753988029933538, 65.06518717409400665, 30.44471234641811819 ) ) ;
#17916 = DIRECTION ( 'NONE',  ( 1.000000000000000000, 0.000000000000000000, 0.000000000000000000 ) ) ;
#17917 = EDGE_CURVE ( 'NONE', #13462, #9830, #14467, .T. ) ;
#17918 = CARTESIAN_POINT ( 'NONE',  ( -154.3824083646099439, -167.4938272943107336, 40.69124936498395328 ) ) ;
#17919 = CARTESIAN_POINT ( 'NONE',  ( 108.9927164799167372, 227.3511983043831037, -5.999999999999976019 ) ) ;
#17920 = CARTESIAN_POINT ( 'NONE',  ( -141.4692556286852891, -176.9130981290892635, 46.40781461928724383 ) ) ;
#17921 = DIRECTION ( 'NONE',  ( 1.000000000000000000, -0.000000000000000000, -0.000000000000000000 ) ) ;
#17923 = EDGE_CURVE ( 'NONE', #7690, #13353, #21479, .T. ) ;
#17922 = CARTESIAN_POINT ( 'NONE',  ( 43.01140435219951286, 155.0344580088725479, 28.95336869806222779 ) ) ;
#17924 = CARTESIAN_POINT ( 'NONE',  ( 38.58424406990784661, 129.5297705074273154, 35.64915139335016647 ) ) ;
#17925 = CARTESIAN_POINT ( 'NONE',  ( 8.701189160817120793, 119.3880529461122109, 1.073064441167490557 ) ) ;
#17926 = CARTESIAN_POINT ( 'NONE',  ( 44.37947211624943833, 124.0151871740939953, 38.42115945441014446 ) ) ;
#17927 = LINE ( 'NONE', #2837, #14840 ) ;
#17928 = CARTESIAN_POINT ( 'NONE',  ( 46.10157429594899270, 65.66049967264873999, 29.95742577749336988 ) ) ;
#17929 = CARTESIAN_POINT ( 'NONE',  ( 43.01140435219951996, 10.71049967264875491, 29.21067981925357060 ) ) ;
#17930 = CARTESIAN_POINT ( 'NONE',  ( 53.47116958538193643, 146.1823035489369715, 17.34243072007611985 ) ) ;
#17931 = CARTESIAN_POINT ( 'NONE',  ( 48.01140435219951996, 83.36049967264872862, 32.58608133808903773 ) ) ;
#17932 = ORIENTED_EDGE ( 'NONE', *, *, #20457, .F. ) ;
#17933 = EDGE_CURVE ( 'NONE', #12813, #13722, #19095, .T. ) ;
#17934 = CARTESIAN_POINT ( 'NONE',  ( 47.05648932407426344, 85.91049967264873999, 37.14960608071593384 ) ) ;
#17935 = ORIENTED_EDGE ( 'NONE', *, *, #4901, .F. ) ;
#17936 =( BOUNDED_CURVE ( )  B_SPLINE_CURVE ( 2, ( #17713, #20935, #12658, #20717, #3965, #5928, #4376, #7278, #866, #17499, #19379, #652, #12327 ),
 .UNSPECIFIED., .F., .F. ) 
 B_SPLINE_CURVE_WITH_KNOTS ( ( 3, 2, 2, 2, 2, 2, 3 ),
 ( 0.7321428571428572063, 0.7357142857142857650, 0.7428571428571428825, 0.7500000000000000000, 0.7571428571428571175, 0.7642857142857142350, 0.7678571428571427937 ),
 .UNSPECIFIED. ) 
 CURVE ( )  GEOMETRIC_REPRESENTATION_ITEM ( )  RATIONAL_B_SPLINE_CURVE ( ( 0.9755282581475768211, 0.9755282581475771542, 1.000000000000000000, 0.9510565162951535312, 1.000000000000000000, 0.9510565162951535312, 1.000000000000000000, 0.9510565162951535312, 1.000000000000000000, 0.9510565162951535312, 1.000000000000000000, 0.9755282581475771542, 0.9755282581475768211 ) ) 
 REPRESENTATION_ITEM ( '' )  );
#17937 = CARTESIAN_POINT ( 'NONE',  ( 48.01140435219951996, 82.13445800887255643, 35.83527830041810347 ) ) ;
#17938 = PLANE ( 'NONE',  #7021 ) ;
#17939 = CLOSED_SHELL ( 'NONE', ( #11191, #16348, #17636, #2322, #7713, #1036 ) ) ;
#17940 = AXIS2_PLACEMENT_3D ( 'NONE', #13732, #19029, #18809 ) ;
#17941 = CARTESIAN_POINT ( 'NONE',  ( 48.01140435219951996, 146.0604996726487457, 35.83527830041810347 ) ) ;
#17943 = CARTESIAN_POINT ( 'NONE',  ( 51.61786746416480298, 93.13668562621728597, 1.065498654441493720 ) ) ;
#17942 = CARTESIAN_POINT ( 'NONE',  ( 43.01140435219951286, 93.86518717409400381, 38.86567161673127657 ) ) ;
#17944 = EDGE_CURVE ( 'NONE', #706, #3989, #2839, .T. ) ;
#17945 = CARTESIAN_POINT ( 'NONE',  ( -154.3824083646099439, -172.5584106276440366, 58.62277379824867296 ) ) ;
#17946 = CARTESIAN_POINT ( 'NONE',  ( 43.01140435219951286, 67.46049967264873715, 39.46799094044489209 ) ) ;
#17948 = CARTESIAN_POINT ( 'NONE',  ( -154.5594255724347761, -158.1630981290892919, 40.14644641866476604 ) ) ;
#17947 = CARTESIAN_POINT ( 'NONE',  ( 47.97830229121277057, 144.4087953931572201, 33.55020052675504871 ) ) ;
#17949 = CARTESIAN_POINT ( 'NONE',  ( 38.96631938032478359, 106.0104996726487485, 37.14960608071593384 ) ) ;
#17950 = PLANE ( 'NONE',  #6484 ) ;
#17951 = FACE_OUTER_BOUND ( 'NONE', #11742, .T. ) ;
#17952 = CARTESIAN_POINT ( 'NONE',  ( 44.37947211624943833, 64.01518717409400949, 38.42115945441014446 ) ) ;
#17953 = CARTESIAN_POINT ( 'NONE',  ( 43.10205244623161036, 154.1398065127551149, -10.16071067355346358 ) ) ;
#17954 = EDGE_CURVE ( 'NONE', #17427, #12279, #14915, .T. ) ;
#17955 = CARTESIAN_POINT ( 'NONE',  ( 45.74753988029934249, 151.1651871740940010, 37.97664729208901235 ) ) ;
#17956 = CARTESIAN_POINT ( 'NONE',  ( 43.80332655382222384, 94.53738109496902098, 39.21067981925354928 ) ) ;
#17957 = CARTESIAN_POINT ( 'NONE',  ( -145.6429501568359797, -170.9438272943107222, 41.63779006702063867 ) ) ;
#17958 = CARTESIAN_POINT ( 'NONE',  ( -142.0420953463935803, -180.5084106276440536, 46.59394152635518083 ) ) ;
#17959 = ORIENTED_EDGE ( 'NONE', *, *, #88, .T. ) ;
#17960 = CARTESIAN_POINT ( 'NONE',  ( 47.43856463449118621, 70.61518717409400381, 34.21067981925357060 ) ) ;
#17961 = CARTESIAN_POINT ( 'NONE',  ( -142.0420953463935803, -165.8084106276440366, 52.72008163687743831 ) ) ;
#17962 = CARTESIAN_POINT ( 'NONE',  ( 22.02512380705847406, 92.75866610308527527, 21.07306443996510481 ) ) ;
#17963 = DIRECTION ( 'NONE',  ( -1.000000000000000000, 0.000000000000000000, 0.000000000000000000 ) ) ;
#17964 = CARTESIAN_POINT ( 'NONE',  ( 38.58424406990786082, 138.1151871740940180, 34.21067981925357060 ) ) ;
#17965 = AXIS2_PLACEMENT_3D ( 'NONE', #10047, #1876, #3434 ) ;
#17966 = CARTESIAN_POINT ( 'NONE',  ( 76.77449255912956971, 125.0547954796211485, -7.584917068115353267 ) ) ;
#17967 = ORIENTED_EDGE ( 'NONE', *, *, #588, .T. ) ;
#17968 = ORIENTED_EDGE ( 'NONE', *, *, #9359, .T. ) ;
#17969 = VERTEX_POINT ( 'NONE', #20015 ) ;
#17970 = LINE ( 'NONE', #12803, #17104 ) ;
#17971 = ADVANCED_FACE ( 'NONE', ( #13595 ), #15257, .T. ) ;
#17972 = CARTESIAN_POINT ( 'NONE',  ( 43.01140435219951286, 77.62977050742729546, 29.55568802177586463 ) ) ;
#17973 = CARTESIAN_POINT ( 'NONE',  ( 45.74753988029933538, 134.0651871740939498, 30.44471234641811819 ) ) ;
#17974 = CARTESIAN_POINT ( 'NONE',  ( 47.05648932407426344, 89.51049967264873430, 31.27175355779120025 ) ) ;
#17975 = CARTESIAN_POINT ( 'NONE',  ( 73.72238702602700755, 135.0318370961144296, 5.077453337991364002 ) ) ;
#17976 = CARTESIAN_POINT ( 'NONE',  ( -32.30114424549768870, -19.06233958201669410, -35.00000000000000000 ) ) ;
#17977 = CARTESIAN_POINT ( 'NONE',  ( -145.2889157411863721, -163.4391397928654897, 58.16351966513671812 ) ) ;
#17978 = CARTESIAN_POINT ( 'NONE',  ( 39.42975644700377558, 87.41518717409401518, 36.81289934271958941 ) ) ;
#17979 = CARTESIAN_POINT ( 'NONE',  ( 48.01140435219951996, 151.2844580088725763, 34.21067981925357060 ) ) ;
#17980 = CARTESIAN_POINT ( 'NONE',  ( 48.01140435219951996, 109.2844580088725905, 34.21067981925357060 ) ) ;
#17981 = CARTESIAN_POINT ( 'NONE',  ( 43.01140435219951286, 124.4604996726487371, 39.21067981925356349 ) ) ;
#17982 = VERTEX_POINT ( 'NONE', #156 ) ;
#17983 = CARTESIAN_POINT ( 'NONE',  ( 41.64333658814960870, 77.77977050742731535, 30.00020018409699318 ) ) ;
#17984 = CARTESIAN_POINT ( 'NONE',  ( -151.4692556286852891, -193.4084106276440593, 59.56931450028537967 ) ) ;
#17985 = CARTESIAN_POINT ( 'NONE',  ( 11.39584491653312526, 106.7788786240791978, 8.648593811254444930 ) ) ;
#17986 = CARTESIAN_POINT ( 'NONE',  ( -148.5561028927606344, -187.2584106276440536, 58.62277379824867296 ) ) ;
#17987 = ORIENTED_EDGE ( 'NONE', *, *, #21778, .T. ) ;
#17988 = DIRECTION ( 'NONE',  ( 0.000000000000000000, 0.000000000000000000, 1.000000000000000000 ) ) ;
#17989 = CYLINDRICAL_SURFACE ( 'NONE', #6035, 10.00000000000000888 ) ;
#17990 = CARTESIAN_POINT ( 'NONE',  ( 47.43856463449118621, 121.8797705074273239, 34.21067981925357060 ) ) ;
#17991 = ORIENTED_EDGE ( 'NONE', *, *, #3564, .T. ) ;
#17992 = ADVANCED_FACE ( 'NONE', ( #3249 ), #1484, .T. ) ;
#17993 = SURFACE_SIDE_STYLE ('',( #11273 ) ) ;
#17994 = EDGE_LOOP ( 'NONE', ( #3645, #11355, #10427, #18160 ) ) ;
#17995 = CARTESIAN_POINT ( 'NONE',  ( 43.01140435219951286, 128.6297705074273097, 29.55568802177586463 ) ) ;
#17996 = CARTESIAN_POINT ( 'NONE',  ( 41.46631938032478359, 73.31049967264874567, 38.96596240072933170 ) ) ;
#17997 = CARTESIAN_POINT ( 'NONE',  ( 45.74753988029933538, 88.42977050742729261, 37.97664729208901946 ) ) ;
#17998 = CARTESIAN_POINT ( 'NONE',  ( 47.05648932407426344, 64.58445800887258770, 31.27175355779120025 ) ) ;
#17999 = VECTOR ( 'NONE', #13364, 1000.000000000000114 ) ;
#18000 = AXIS2_PLACEMENT_3D ( 'NONE', #3669, #17099, #10610 ) ;
#18001 = LINE ( 'NONE', #3133, #9407 ) ;
#18002 = CARTESIAN_POINT ( 'NONE',  ( 43.01140435219951286, 101.0344580088725621, 29.21067981925356705 ) ) ;
#18003 = CARTESIAN_POINT ( 'NONE',  ( 0.08333186253067781379, 634.6318465664365931, -19.99999999999997868 ) ) ;
#18004 = CARTESIAN_POINT ( 'NONE',  ( -151.4692556286852891, -192.2391397928654726, 39.14238933923362396 ) ) ;
#18005 = DIRECTION ( 'NONE',  ( -0.000000000000000000, 1.000000000000000000, -0.000000000000000000 ) ) ;
#18006 = CARTESIAN_POINT ( 'NONE',  ( 45.22504609509771001, 59.11591859955431971, 30.37668211462113277 ) ) ;
#18007 = CARTESIAN_POINT ( 'NONE',  ( -142.0420953463935803, -192.5438272943107449, 52.72008163687743831 ) ) ;
#18008 = PRODUCT_CONTEXT ( 'NONE', #1833, 'mechanical' ) ;
#18009 = AXIS2_PLACEMENT_3D ( 'NONE', #18802, #3707, #10222 ) ;
#18010 = CARTESIAN_POINT ( 'NONE',  ( 43.01140435219951286, 120.5344580088725763, 39.46799094044489209 ) ) ;
#18011 = CARTESIAN_POINT ( 'NONE',  ( 39.42975644700377558, 99.67977050742732104, 36.81289934271958941 ) ) ;
#18012 = CARTESIAN_POINT ( 'NONE',  ( 14.73996261871784341, 120.6514404024884755, 15.19984638209844441 ) ) ;
#18013 = CARTESIAN_POINT ( 'NONE',  ( -143.8425227516148084, -186.0938272943107279, 44.11586579668791330 ) ) ;
#18014 = CARTESIAN_POINT ( 'NONE',  ( 43.01140435219951286, 99.86518717409401802, 38.86567161673127657 ) ) ;
#18015 = CARTESIAN_POINT ( 'NONE',  ( -151.4692556286852891, -178.7391397928654726, 59.65701158161631668 ) ) ;
#18016 = ORIENTED_EDGE ( 'NONE', *, *, #5675, .T. ) ;
#18017 = CARTESIAN_POINT ( 'NONE',  ( 43.01140435219951996, 10.71049967264875491, 34.21067981925357060 ) ) ;
#18018 = CARTESIAN_POINT ( 'NONE',  ( 73.72238702602700755, 135.0318370961144296, 5.077453337991364002 ) ) ;
#18019 = CARTESIAN_POINT ( 'NONE',  ( 41.64333658814960870, 144.9797705074273324, 38.42115945441014446 ) ) ;
#18020 = CARTESIAN_POINT ( 'NONE',  ( 70.22564533444385404, 112.8265553529472953, -14.05338489394683243 ) ) ;
#18021 = ADVANCED_FACE ( 'NONE', ( #5230 ), #1913, .F. ) ;
#18022 = PRODUCT_DEFINITION_SHAPE ( 'NONE', 'NONE',  #21820 ) ;
#18023 = VECTOR ( 'NONE', #14527, 1000.000000000000000 ) ;
#18024 = CARTESIAN_POINT ( 'NONE',  ( 46.59305225739526435, 67.57977050742732672, 36.81289934271958941 ) ) ;
#18025 = ORIENTED_EDGE ( 'NONE', *, *, #8065, .T. ) ;
#18026 = EDGE_LOOP ( 'NONE', ( #13694, #17747, #19102, #896 ) ) ;
#18027 = CARTESIAN_POINT ( 'NONE',  ( 47.43856463449117200, 158.0297705074273438, 32.77220824515698183 ) ) ;
#18028 = CARTESIAN_POINT ( 'NONE',  ( -151.4692556286852891, -177.8130981290892976, 59.65701158161631668 ) ) ;
#18029 = EDGE_CURVE ( 'NONE', #11386, #706, #8216, .T. ) ;
#18030 = CARTESIAN_POINT ( 'NONE',  ( 44.55648932407425633, 113.8104996726487457, 29.45539723777780239 ) ) ;
#18031 = CARTESIAN_POINT ( 'NONE',  ( 39.42975644700377558, 65.81518717409400665, 31.60846029578754468 ) ) ;
#18032 = CARTESIAN_POINT ( 'NONE',  ( -142.0420953463936087, -156.6584106276440593, 49.65701158161630957 ) ) ;
#18033 = CARTESIAN_POINT ( 'NONE',  ( -151.4692556286852891, -164.6438272943107108, 39.74470866294723947 ) ) ;
#18034 = CARTESIAN_POINT ( 'NONE',  ( -149.8854112254399809, -165.3160212151857138, 39.65701158161628825 ) ) ;
#18035 = CARTESIAN_POINT ( 'NONE',  ( -161.4692556286852607, -175.7130981290893317, 46.40781461928724383 ) ) ;
#18036 = CARTESIAN_POINT ( 'NONE',  ( 38.01140435219952707, 152.7844580088725763, 34.21067981925357060 ) ) ;
#18037 = CARTESIAN_POINT ( 'NONE',  ( 43.01140435219951286, 131.6297705074273381, 29.55568802177586463 ) ) ;
#18038 = CARTESIAN_POINT ( 'NONE',  ( 35.88495058779732716, 86.34054347403214535, 13.57279861601404036 ) ) ;
#18039 = CARTESIAN_POINT ( 'NONE',  ( 46.59305225739526435, 127.9151871740940010, 31.60846029578754468 ) ) ;
#18040 = DIRECTION ( 'NONE',  ( -0.000000000000000000, -0.000000000000000000, -1.000000000000000000 ) ) ;
#18041 = CARTESIAN_POINT ( 'NONE',  ( -148.5561028927606344, -156.0584106276440650, 40.69124936498395328 ) ) ;
#18042 = FACE_OUTER_BOUND ( 'NONE', #14178, .T. ) ;
#18043 = CARTESIAN_POINT ( 'NONE',  ( 43.80332655382220963, 148.5373810949689926, 39.21067981925356349 ) ) ;
#18044 = CARTESIAN_POINT ( 'NONE',  ( 51.94691807752363388, 146.6530262932614050, -9.724486432582017059 ) ) ;
#18045 = CARTESIAN_POINT ( 'NONE',  ( -143.3790856849358306, -187.2891397928654555, 55.53486410454105027 ) ) ;
#18046 = ORIENTED_EDGE ( 'NONE', *, *, #15126, .F. ) ;
#18047 = CARTESIAN_POINT ( 'NONE',  ( -101.1064508287285832, 10.96617311717548660, 4.000000000000021316 ) ) ;
#18048 = ORIENTED_EDGE ( 'NONE', *, *, #14083, .F. ) ;
#18049 = CARTESIAN_POINT ( 'NONE',  ( 38.01140435219952707, 80.78445800887257633, 34.21067981925357060 ) ) ;
#18050 = DIRECTION ( 'NONE',  ( 0.000000000000000000, 0.000000000000000000, -1.000000000000000000 ) ) ;
#18051 = CARTESIAN_POINT ( 'NONE',  ( 44.55648932407425633, 139.6104996726487286, 38.96596240072933170 ) ) ;
#18053 = CARTESIAN_POINT ( 'NONE',  ( 36.14055301128134801, 147.1744539460121075, 4.637215583376333328 ) ) ;
#18052 = CARTESIAN_POINT ( 'NONE',  ( 47.43856463449117200, 94.46518717409398391, 35.64915139335016647 ) ) ;
#18054 = DIRECTION ( 'NONE',  ( 0.000000000000000000, 0.000000000000000000, -1.000000000000000000 ) ) ;
#18055 = CARTESIAN_POINT ( 'NONE',  ( -148.5561028927606344, -163.2584106276440536, 58.62277379824867296 ) ) ;
#18056 = EDGE_CURVE ( 'NONE', #13533, #9454, #15371, .T. ) ;
#18057 = CARTESIAN_POINT ( 'NONE',  ( 39.92123440845004723, 66.26049967264874851, 29.95742577749337343 ) ) ;
#18059 = DIRECTION ( 'NONE',  ( 1.000000000000000000, 0.000000000000000000, 0.000000000000000000 ) ) ;
#18058 = CARTESIAN_POINT ( 'NONE',  ( -153.0531000319306543, -177.8899795514095388, 59.65701158161632378 ) ) ;
#18060 = CARTESIAN_POINT ( 'NONE',  ( 43.01140435219951286, 106.4604996726487371, 39.21067981925356349 ) ) ;
#18061 = CARTESIAN_POINT ( 'NONE',  ( -151.4692556286852891, -176.3130981290892976, 39.65701158161629536 ) ) ;
#18062 = CARTESIAN_POINT ( 'NONE',  ( 44.55648932407425633, 145.6104996726487570, 38.96596240072933170 ) ) ;
#18063 = ADVANCED_FACE ( 'NONE', ( #3577 ), #10304, .T. ) ;
#18064 = CARTESIAN_POINT ( 'NONE',  ( 46.59305225739526435, 158.1797705074273210, 31.60846029578754468 ) ) ;
#18065 = CARTESIAN_POINT ( 'NONE',  ( 77.19215121279506775, 118.0176990621192203, -1.351406188750652992 ) ) ;
#18066 = CARTESIAN_POINT ( 'NONE',  ( 39.42975644700377558, 152.8151871740940067, 31.60846029578754468 ) ) ;
#18067 = CARTESIAN_POINT ( 'NONE',  ( -142.0420953463935803, -168.5438272943107165, 52.72008163687743831 ) ) ;
#18068 = CARTESIAN_POINT ( 'NONE',  ( -157.2955611005345986, -184.7084106276440423, 57.67623309621197336 ) ) ;
#18069 = VERTEX_POINT ( 'NONE', #15144 ) ;
#18070 = CARTESIAN_POINT ( 'NONE',  ( 41.64333658814960870, 72.71518717409399812, 38.42115945441014446 ) ) ;
#18071 = CARTESIAN_POINT ( 'NONE',  ( -151.4692556286852891, -170.9084106276440593, 39.74470866294723947 ) ) ;
#18072 = CARTESIAN_POINT ( 'NONE',  ( 68.49994877969884044, 96.93213776073638144, 19.40600457995573080 ) ) ;
#18073 = CARTESIAN_POINT ( 'NONE',  ( -81.61981105773979550, 604.5992151483073940, -0.8325491102011938205 ) ) ;
#18074 = CARTESIAN_POINT ( 'NONE',  ( 39.42975644700377558, 137.8151871740940067, 31.60846029578754468 ) ) ;
#18075 = CARTESIAN_POINT ( 'NONE',  ( 30.47730968207189051, 151.6776658675815384, -2.585197649422186661 ) ) ;
#18076 =( BOUNDED_CURVE ( )  B_SPLINE_CURVE ( 2, ( #18840, #15531, #17391, #3746, #10257, #17066, #10578, #15432, #9035, #15321, #18952, #10476, #5491 ),
 .UNSPECIFIED., .F., .F. ) 
 B_SPLINE_CURVE_WITH_KNOTS ( ( 3, 2, 2, 2, 2, 2, 3 ),
 ( 0.1607142857142856707, 0.1642857142857142849, 0.1714285714285714302, 0.1785714285714285754, 0.1857142857142857206, 0.1928571428571428659, 0.1964285714285714524 ),
 .UNSPECIFIED. ) 
 CURVE ( )  GEOMETRIC_REPRESENTATION_ITEM ( )  RATIONAL_B_SPLINE_CURVE ( ( 0.9755282581475765991, 0.9755282581475763770, 1.000000000000000000, 0.9510565162951535312, 1.000000000000000000, 0.9510565162951535312, 1.000000000000000000, 0.9510565162951535312, 1.000000000000000000, 0.9510565162951535312, 1.000000000000000000, 0.9755282581475765991, 0.9755282581475767101 ) ) 
 REPRESENTATION_ITEM ( '' )  );
#18077 = ORIENTED_EDGE ( 'NONE', *, *, #7363, .F. ) ;
#18078 = ORIENTED_EDGE ( 'NONE', *, *, #14083, .T. ) ;
#18079 = AXIS2_PLACEMENT_3D ( 'NONE', #6114, #7789, #17474 ) ;
#18080 = CARTESIAN_POINT ( 'NONE',  ( 71.07552608251525328, 117.1481954606975791, 12.77539325861266484 ) ) ;
#18081 = ORIENTED_EDGE ( 'NONE', *, *, #13428, .F. ) ;
#18082 = CARTESIAN_POINT ( 'NONE',  ( 48.01140435219951996, 116.3604996726487286, 32.58608133808903773 ) ) ;
#18083 = CARTESIAN_POINT ( 'NONE',  ( 43.01140435219951286, 68.62977050742729546, 29.55568802177586463 ) ) ;
#18085 = CARTESIAN_POINT ( 'NONE',  ( 49.55020742284296631, 92.47612394764220767, 0.1565338505643876776 ) ) ;
#18084 = CARTESIAN_POINT ( 'NONE',  ( 39.42975644700377558, 123.4151871740940010, 36.81289934271958941 ) ) ;
#18086 = VECTOR ( 'NONE', #2083, 1000.000000000000000 ) ;
#18087 = CARTESIAN_POINT ( 'NONE',  ( 39.92123440845004723, 96.26049967264873430, 29.95742577749337343 ) ) ;
#18088 = CYLINDRICAL_SURFACE ( 'NONE', #18518, 7.500000000000007105 ) ;
#18089 = CARTESIAN_POINT ( 'NONE',  ( 43.01140435219951996, 10.71049967264875491, 34.21067981925357060 ) ) ;
#18090 = FACE_OUTER_BOUND ( 'NONE', #16448, .T. ) ;
#18091 = CARTESIAN_POINT ( 'NONE',  ( 45.74753988029933538, 85.16518717409400097, 37.97664729208901946 ) ) ;
#18092 = DIRECTION ( 'NONE',  ( 0.3428981916074309577, -0.9393725726208709270, 0.000000000000000000 ) ) ;
#18093 = LINE ( 'NONE', #21420, #2874 ) ;
#18094 = ORIENTED_EDGE ( 'NONE', *, *, #3602, .F. ) ;
#18095 = CARTESIAN_POINT ( 'NONE',  ( 41.64333658814960870, 74.77977050742731535, 30.00020018409699318 ) ) ;
#18096 = CARTESIAN_POINT ( 'NONE',  ( -157.2955611005346270, -191.6084106276440764, 41.63779006702063867 ) ) ;
#18097 = CARTESIAN_POINT ( 'NONE',  ( 20.88913110926514705, 146.0313881486468119, 3.053432864643822686 ) ) ;
#18098 = CARTESIAN_POINT ( 'NONE',  ( -154.3824083646099439, -181.5584106276440650, 58.62277379824867296 ) ) ;
#18099 = VERTEX_POINT ( 'NONE', #5015 ) ;
#18100 = CARTESIAN_POINT ( 'NONE',  ( -151.4692556286852891, -196.9891397928655010, 49.65701158161630957 ) ) ;
#18101 = ADVANCED_FACE ( 'NONE', ( #6999 ), #17006, .F. ) ;
#18102 = CARTESIAN_POINT ( 'NONE',  ( 162.3411339277076308, 184.7625696037766261, 4.000000000000003553 ) ) ;
#18103 = ADVANCED_FACE ( 'NONE', ( #8323 ), #20439, .T. ) ;
#18104 = AXIS2_PLACEMENT_3D ( 'NONE', #15671, #3894, #16071 ) ;
#18105 = CARTESIAN_POINT ( 'NONE',  ( 40.27526882409969744, 120.8297705074273125, 37.97664729208901235 ) ) ;
#18106 = ORIENTED_EDGE ( 'NONE', *, *, #5672, .F. ) ;
#18107 = CARTESIAN_POINT ( 'NONE',  ( 43.80332655382220253, 88.95757658655229250, 29.21067981925356705 ) ) ;
#18108 = ORIENTED_EDGE ( 'NONE', *, *, #10158, .T. ) ;
#18109 = CARTESIAN_POINT ( 'NONE',  ( 38.96631938032478359, 72.41049967264873999, 31.27175355779120025 ) ) ;
#18110 = CARTESIAN_POINT ( 'NONE',  ( 40.27526882409969033, 152.6651871740940010, 30.44471234641811819 ) ) ;
#18111 = LINE ( 'NONE', #20013, #15735 ) ;
#18112 = DIRECTION ( 'NONE',  ( -1.000000000000000000, 0.000000000000000000, 0.000000000000000000 ) ) ;
#18113 =( NAMED_UNIT ( * ) SI_UNIT ( $, .STERADIAN. ) SOLID_ANGLE_UNIT ( ) );
#18114 = CARTESIAN_POINT ( 'NONE',  ( -141.4692556286852891, -192.8391397928654669, 46.40781461928724383 ) ) ;
#18115 = CARTESIAN_POINT ( 'NONE',  ( 43.01140435219951286, 73.46049967264872294, 39.21067981925356349 ) ) ;
#18116 = CARTESIAN_POINT ( 'NONE',  ( -151.4692556286852891, -196.9891397928655010, 49.65701158161630957 ) ) ;
#18117 = CARTESIAN_POINT ( 'NONE',  ( -145.6429501568359797, -189.8438272943106995, 57.67623309621198047 ) ) ;
#18118 = ADVANCED_FACE ( 'NONE', ( #13280 ), #9866, .F. ) ;
#18119 = CARTESIAN_POINT ( 'NONE',  ( 44.55648932407425633, 118.8844580088725849, 29.45539723777780239 ) ) ;
#18120 = CARTESIAN_POINT ( 'NONE',  ( 47.43856463449117200, 103.7297705074273182, 35.64915139335016647 ) ) ;
#18121 = CARTESIAN_POINT ( 'NONE',  ( 14.82355424275916000, 117.6079223783217458, 15.08068057431173870 ) ) ;
#18122 = CARTESIAN_POINT ( 'NONE',  ( -157.2955611005346270, -179.3438272943107279, 41.63779006702063867 ) ) ;
#18123 = CARTESIAN_POINT ( 'NONE',  ( 38.58424406990785371, 89.96518717409399812, 32.77220824515697473 ) ) ;
#18124 = DIRECTION ( 'NONE',  ( 0.000000000000000000, -1.000000000000000000, 0.000000000000000000 ) ) ;
#18125 = VECTOR ( 'NONE', #10235, 1000.000000000000000 ) ;
#18126 = VERTEX_POINT ( 'NONE', #16900 ) ;
#18127 = DIRECTION ( 'NONE',  ( -0.000000000000000000, 1.000000000000000000, -0.000000000000000000 ) ) ;
#18128 = CARTESIAN_POINT ( 'NONE',  ( 72.33162239183086228, 137.5781058455011703, 11.98183203572534872 ) ) ;
#18129 = CARTESIAN_POINT ( 'NONE',  ( 37.89917375590665927, 147.5588116854153498, -9.291614562240097186 ) ) ;
#18130 = CARTESIAN_POINT ( 'NONE',  ( 44.37947211624943833, 68.47977050742731819, 30.00020018409699318 ) ) ;
#18131 = B_SPLINE_CURVE_WITH_KNOTS ( 'NONE', 3,
 ( #4709, #11427, #8138, #4820 ),
 .UNSPECIFIED., .F., .F.,
 ( 4, 4 ),
 ( 0.000000000000000000, 1.000000000000000000 ),
 .UNSPECIFIED. ) ;
#18132 = ORIENTED_EDGE ( 'NONE', *, *, #4408, .T. ) ;
#18133 = ORIENTED_EDGE ( 'NONE', *, *, #20409, .T. ) ;
#18134 = CARTESIAN_POINT ( 'NONE',  ( 44.37947211624943833, 146.4797705074273324, 30.00020018409699318 ) ) ;
#18135 =( BOUNDED_CURVE ( )  B_SPLINE_CURVE ( 2, ( #17216, #18883, #3792, #2134, #8866, #15574, #13914, #10624, #5536, #15677, #581, #14350, #6303 ),
 .UNSPECIFIED., .F., .F. ) 
 B_SPLINE_CURVE_WITH_KNOTS ( ( 3, 2, 2, 2, 2, 2, 3 ),
 ( 0.9632352941176470784, 0.9647058823529411908, 0.9676470588235294157, 0.9705882352941176405, 0.9735294117647058654, 0.9764705882352940902, 0.9779411764705882026 ),
 .UNSPECIFIED. ) 
 CURVE ( )  GEOMETRIC_REPRESENTATION_ITEM ( )  RATIONAL_B_SPLINE_CURVE ( ( 0.9755282581475768211, 0.9755282581475768211, 1.000000000000000000, 0.9510565162951535312, 1.000000000000000000, 0.9510565162951535312, 1.000000000000000000, 0.9510565162951535312, 1.000000000000000000, 0.9510565162951535312, 1.000000000000000000, 0.9755282581475768211, 0.9755282581475768211 ) ) 
 REPRESENTATION_ITEM ( '' )  );
#18136 = CARTESIAN_POINT ( 'NONE',  ( -151.4692556286852891, -176.3130981290892976, 39.65701158161629536 ) ) ;
#18137 = VECTOR ( 'NONE', #20950, 1000.000000000000000 ) ;
#18138 = CARTESIAN_POINT ( 'NONE',  ( 43.01140435219951286, 109.4604996726487514, 39.46799094044489209 ) ) ;
#18139 = CARTESIAN_POINT ( 'NONE',  ( 39.42975644700377558, 68.81518717409400665, 31.60846029578754468 ) ) ;
#18140 = CARTESIAN_POINT ( 'NONE',  ( 38.96631938032478359, 65.48445800887257917, 31.27175355779120025 ) ) ;
#18141 = CARTESIAN_POINT ( 'NONE',  ( -142.0420953463936087, -159.3938272943107393, 49.65701158161630957 ) ) ;
#18142 = CARTESIAN_POINT ( 'NONE',  ( 163.3355671671241680, 191.7371538283428265, 21.25714143325154026 ) ) ;
#18143 = CARTESIAN_POINT ( 'NONE',  ( -143.3790856849358306, -174.3630981290893089, 55.53486410454105027 ) ) ;
#18144 = EDGE_CURVE ( 'NONE', #7658, #417, #16682, .T. ) ;
#18145 = CARTESIAN_POINT ( 'NONE',  ( 42.21948215057684450, 112.3836182503284675, 39.21067981925355639 ) ) ;
#18146 = CARTESIAN_POINT ( 'NONE',  ( 47.05648932407426344, 147.9844580088725934, 37.14960608071593384 ) ) ;
#18147 = CARTESIAN_POINT ( 'NONE',  ( 46.59305225739526435, 128.1797705074273210, 31.60846029578754468 ) ) ;
#18148 = CARTESIAN_POINT ( 'NONE',  ( 45.08439497331802670, 154.1588294112744677, 16.90626985941621641 ) ) ;
#18149 = CARTESIAN_POINT ( 'NONE',  ( 46.59305225739526435, 112.9151871740940010, 31.60846029578754468 ) ) ;
#18150 = DIRECTION ( 'NONE',  ( -0.000000000000000000, 1.000000000000000000, -0.000000000000000000 ) ) ;
#18151 = CARTESIAN_POINT ( 'NONE',  ( -145.6429501568359797, -157.1084106276440480, 57.67623309621197336 ) ) ;
#18152 = CIRCLE ( 'NONE', #8670, 14.42424326798555434 ) ;
#18153 = CARTESIAN_POINT ( 'NONE',  ( -136.4581486297550441, -116.9891397928655010, 49.65701158161631668 ) ) ;
#18154 = CARTESIAN_POINT ( 'NONE',  ( 46.10157429594899270, 148.7604996726487627, 38.46393386101375711 ) ) ;
#18155 = CARTESIAN_POINT ( 'NONE',  ( 17.64326796073342862, 132.3496329740814303, 22.67862939001841127 ) ) ;
#18156 = CARTESIAN_POINT ( 'NONE',  ( 38.96631938032478359, 120.4104996726487400, 31.27175355779120025 ) ) ;
#18157 = CARTESIAN_POINT ( 'NONE',  ( 45.74753988029934249, 98.32977050742731251, 30.44471234641812174 ) ) ;
#18158 = EDGE_LOOP ( 'NONE', ( #19353, #16067, #2415, #12420, #57, #20749, #4640, #699, #14118, #15388, #7738, #8751, #5746, #20295, #7581, #10512, #15755, #5581, #1009, #2392, #1439, #19099, #14766, #19600, #19541, #21157, #13899, #17967, #20691, #7528, #20832, #5638, #5822, #4580, #14227, #9455, #11239, #4412, #19010, #4334, #1170, #4634, #18521, #12171, #18016, #4311, #14204, #21406, #16638, #11086, #15214, #2844, #15557, #3454, #19258, #357, #9311, #12931, #8878, #9537, #18278, #9779, #2739, #11142, #12771, #3663, #14502, #7195, #16344, #4309, #18686 ) ) ;
#18159 = DIRECTION ( 'NONE',  ( -0.5000000000000004441, 0.000000000000000000, -0.8660254037844383745 ) ) ;
#18160 = ORIENTED_EDGE ( 'NONE', *, *, #1837, .F. ) ;
#18161 = CARTESIAN_POINT ( 'NONE',  ( 44.55648932407425633, 85.88445800887258486, 29.45539723777780239 ) ) ;
#18162 = DIRECTION ( 'NONE',  ( 0.000000000000000000, 0.000000000000000000, 1.000000000000000000 ) ) ;
#18163 = CARTESIAN_POINT ( 'NONE',  ( 38.01140435219951996, 135.8604996726487002, 35.83527830041810347 ) ) ;
#18165 = CARTESIAN_POINT ( 'NONE',  ( 65.51498131554875215, 136.7693945797108199, 5.946615082358765569 ) ) ;
#18164 = CARTESIAN_POINT ( 'NONE',  ( 38.58424406990784661, 96.26518717409400949, 35.64915139335016647 ) ) ;
#18166 = LINE ( 'NONE', #3074, #9147 ) ;
#18167 = CARTESIAN_POINT ( 'NONE',  ( -148.5561028927606344, -165.0584106276440366, 40.69124936498395328 ) ) ;
#18168 = ADVANCED_FACE ( 'NONE', ( #20122 ), #11723, .T. ) ;
#18169 = CARTESIAN_POINT ( 'NONE',  ( -154.3824083646099439, -190.2938272943107449, 58.62277379824867296 ) ) ;
#18171 = DIRECTION ( 'NONE',  ( -1.000000000000000000, 0.000000000000000000, 1.723963091245776092E-16 ) ) ;
#18170 = CARTESIAN_POINT ( 'NONE',  ( -176.9699209214867324, -126.9891397928655010, -72.64809332337415526 ) ) ;
#18172 = CARTESIAN_POINT ( 'NONE',  ( -27.64582385433943656, -34.13255853780189142, 20.00000000000001776 ) ) ;
#18173 = VECTOR ( 'NONE', #2733, 1000.000000000000114 ) ;
#18174 = CARTESIAN_POINT ( 'NONE',  ( -145.2889157411863437, -175.4391397928654328, 58.16351966513671812 ) ) ;
#18175 = CARTESIAN_POINT ( 'NONE',  ( 43.80332655382220253, 114.6113394311928317, 39.21067981925355639 ) ) ;
#18176 = AXIS2_PLACEMENT_3D ( 'NONE', #16676, #13489, #5114 ) ;
#18177 = CARTESIAN_POINT ( 'NONE',  ( 45.74753988029933538, 62.06518717409399244, 30.44471234641811819 ) ) ;
#18178 = CARTESIAN_POINT ( 'NONE',  ( 38.01140435219952707, 62.63445800887255643, 32.58608133808903773 ) ) ;
#18179 = CARTESIAN_POINT ( 'NONE',  ( 50.92548328124963319, 86.60151408976496157, 0.07716523989554470442 ) ) ;
#18180 = CARTESIAN_POINT ( 'NONE',  ( 47.43856463449118621, 145.6151871740939896, 34.21067981925357060 ) ) ;
#18181 = CARTESIAN_POINT ( 'NONE',  ( -160.8964159109769696, -158.0438272943107165, 46.59394152635518793 ) ) ;
#18182 = CARTESIAN_POINT ( 'NONE',  ( -142.0420953463935803, -186.5084106276440536, 46.59394152635518083 ) ) ;
#18183 = ORIENTED_EDGE ( 'NONE', *, *, #2798, .T. ) ;
#18184 = CARTESIAN_POINT ( 'NONE',  ( 38.58424406990786082, 69.11518717409400381, 34.21067981925357060 ) ) ;
#18185 = CARTESIAN_POINT ( 'NONE',  ( -154.3824083646099439, -170.7584106276440536, 40.69124936498395328 ) ) ;
#18186 = CARTESIAN_POINT ( 'NONE',  ( 9.116869730174032682, 125.2576736736073428, 22.26325814793822744 ) ) ;
#18187 = DIRECTION ( 'NONE',  ( 0.9385982292947087080, 0.3450121214752279730, 0.000000000000000000 ) ) ;
#18188 = CARTESIAN_POINT ( 'NONE',  ( 47.43856463449117200, 127.4651871740940123, 35.64915139335016647 ) ) ;
#18189 = CARTESIAN_POINT ( 'NONE',  ( 11.65896226128411683, 106.3627486108568547, -4.370744638174604013 ) ) ;
#18190 = CIRCLE ( 'NONE', #11871, 10.00000000000000888 ) ;
#18191 = ORIENTED_EDGE ( 'NONE', *, *, #18659, .F. ) ;
#18192 = ORIENTED_EDGE ( 'NONE', *, *, #3680, .F. ) ;
#18193 = CARTESIAN_POINT ( 'NONE',  ( 27.67177345608778793, 143.5689829720894011, 10.27550654291302479 ) ) ;
#18194 = ORIENTED_EDGE ( 'NONE', *, *, #17717, .F. ) ;
#18195 = CARTESIAN_POINT ( 'NONE',  ( 41.46631938032478359, 108.3844580088725849, 38.96596240072933170 ) ) ;
#18196 = DIRECTION ( 'NONE',  ( 0.000000000000000000, 1.000000000000000000, 0.000000000000000000 ) ) ;
#18197 = CARTESIAN_POINT ( 'NONE',  ( 41.64333658814960870, 62.77977050742732246, 30.00020018409699318 ) ) ;
#18199 = CARTESIAN_POINT ( 'NONE',  ( 62.17156016504299032, 99.21662021101468554, 6.584824431686855384 ) ) ;
#18198 = CARTESIAN_POINT ( 'NONE',  ( 44.37947211624943833, 122.2151871740940123, 30.00020018409699318 ) ) ;
#18200 = CARTESIAN_POINT ( 'NONE',  ( 47.05648932407426344, 83.51049967264874851, 31.27175355779120025 ) ) ;
#18201 = CARTESIAN_POINT ( 'NONE',  ( 28.07864021081662287, 89.10199518432737875, 14.83897397183228861 ) ) ;
#18202 = LINE ( 'NONE', #4755, #6125 ) ;
#18203 = CARTESIAN_POINT ( 'NONE',  ( -143.7724355939531904, 531.4176628826018032, 4.000000000000021316 ) ) ;
#18204 = CARTESIAN_POINT ( 'NONE',  ( 47.43856463449117200, 85.76518717409398107, 32.77220824515698183 ) ) ;
#18205 = CARTESIAN_POINT ( 'NONE',  ( 43.01140435219951286, 106.4604996726487371, 39.21067981925356349 ) ) ;
#18206 = PRODUCT_DEFINITION_SHAPE ( 'NONE', 'NONE',  #21826 ) ;
#18207 = CARTESIAN_POINT ( 'NONE',  ( 46.10157429594899270, 142.7344580088725650, 29.95742577749336988 ) ) ;
#18208 = EDGE_CURVE ( 'NONE', #10265, #5468, #16793, .T. ) ;
#18209 = ORIENTED_EDGE ( 'NONE', *, *, #20245, .F. ) ;
#18210 = CARTESIAN_POINT ( 'NONE',  ( 41.64333658814960870, 68.77977050742731535, 30.00020018409699318 ) ) ;
#18211 =( BOUNDED_CURVE ( )  B_SPLINE_CURVE ( 2, ( #20154, #15067, #4399, #21285, #11647, #2756, #887, #16088, #1213, #21170, #21804, #7735, #1106 ),
 .UNSPECIFIED., .F., .F. ) 
 B_SPLINE_CURVE_WITH_KNOTS ( ( 3, 2, 2, 2, 2, 2, 3 ),
 ( 0.4338235294117647189, 0.4352941176470588314, 0.4382352941176470562, 0.4411764705882352811, 0.4441176470588235059, 0.4470588235294117863, 0.4485294117647058987 ),
 .UNSPECIFIED. ) 
 CURVE ( )  GEOMETRIC_REPRESENTATION_ITEM ( )  RATIONAL_B_SPLINE_CURVE ( ( 0.9755282581475768211, 0.9755282581475768211, 1.000000000000000000, 0.9510565162951535312, 1.000000000000000000, 0.9510565162951535312, 1.000000000000000000, 0.9510565162951535312, 1.000000000000000000, 0.9510565162951535312, 1.000000000000000000, 0.9755282581475768211, 0.9755282581475768211 ) ) 
 REPRESENTATION_ITEM ( '' )  );
#18212 = CARTESIAN_POINT ( 'NONE',  ( -145.6429501568359797, -195.2084106276440707, 41.63779006702063867 ) ) ;
#18213 = CARTESIAN_POINT ( 'NONE',  ( 13.33420504782278293, 102.8437529505761603, 1.505736668420971869 ) ) ;
#18214 = CARTESIAN_POINT ( 'NONE',  ( -143.8425227516148084, -186.9584106276440423, 55.19815736654470584 ) ) ;
#18215 = ORIENTED_EDGE ( 'NONE', *, *, #7644, .F. ) ;
#18216 = CARTESIAN_POINT ( 'NONE',  ( 111.4021762516569964, 137.5714195593754710, 4.000000000000003553 ) ) ;
#18217 = FACE_OUTER_BOUND ( 'NONE', #20374, .T. ) ;
#18218 = CARTESIAN_POINT ( 'NONE',  ( 41.64333658814960870, 114.9797705074273324, 38.42115945441014446 ) ) ;
#18219 = CARTESIAN_POINT ( 'NONE',  ( 15.75986397150585816, 99.18880659646561071, -5.637120474378671808 ) ) ;
#18220 = VECTOR ( 'NONE', #15487, 1000.000000000000000 ) ;
#18221 = ORIENTED_EDGE ( 'NONE', *, *, #12332, .T. ) ;
#18222 = PRODUCT_RELATED_PRODUCT_CATEGORY ( 'part', '', ( #6419 ) ) ;
#18223 = CARTESIAN_POINT ( 'NONE',  ( 111.4021762516569964, 137.5714195593754710, 14.00000000000001776 ) ) ;
#18224 = EDGE_LOOP ( 'NONE', ( #2013, #5223, #21483, #18792 ) ) ;
#18225 = CARTESIAN_POINT ( 'NONE',  ( 40.27526882409969033, 116.9297705074273210, 30.44471234641811819 ) ) ;
#18226 = CIRCLE ( 'NONE', #14694, 10.00000000000000888 ) ;
#18227 = DIRECTION ( 'NONE',  ( 0.2803088796301150820, -0.9599098561846886035, 0.000000000000000000 ) ) ;
#18228 = EDGE_CURVE ( 'NONE', #8397, #5468, #10368, .T. ) ;
#18229 = CARTESIAN_POINT ( 'NONE',  ( 47.43856463449118621, 85.87977050742730967, 34.21067981925357060 ) ) ;
#18230 = CARTESIAN_POINT ( 'NONE',  ( 39.42975644700377558, 150.4151871740940010, 36.81289934271958941 ) ) ;
#18231 = CARTESIAN_POINT ( 'NONE',  ( -156.4692748966155591, -155.6811984188981057, 40.99676866812693277 ) ) ;
#18232 = DIRECTION ( 'NONE',  ( 0.000000000000000000, 0.000000000000000000, 1.000000000000000000 ) ) ;
#18233 = CARTESIAN_POINT ( 'NONE',  ( -70.94676665037205510, 193.0091883945745792, 0.000000000000000000 ) ) ;
#18234 = CARTESIAN_POINT ( 'NONE',  ( -161.4692556286853176, -179.4891397928654726, 49.65701158161630957 ) ) ;
#18235 = ADVANCED_FACE ( 'NONE', ( #10733 ), #14128, .T. ) ;
#18236 = CARTESIAN_POINT ( 'NONE',  ( 38.01140435219952707, 89.93445800887256780, 35.83527830041809636 ) ) ;
#18237 = CARTESIAN_POINT ( 'NONE',  ( 48.01140435219951996, 94.43445800887256780, 32.58608133808903773 ) ) ;
#18238 = CARTESIAN_POINT ( 'NONE',  ( -160.8964159109769696, -193.8938272943107393, 49.65701158161630957 ) ) ;
#18239 = CARTESIAN_POINT ( 'NONE',  ( 48.01140435219951996, 124.2844580088725905, 34.21067981925357060 ) ) ;
#18240 = CARTESIAN_POINT ( 'NONE',  ( 40.27526882409969033, 93.82977050742731251, 37.97664729208901946 ) ) ;
#18241 = CARTESIAN_POINT ( 'NONE',  ( 40.03295031927941494, 147.9482203214073479, -10.20071078494585670 ) ) ;
#18242 = CARTESIAN_POINT ( 'NONE',  ( -148.5561028927606344, -185.7938272943107449, 40.69124936498395328 ) ) ;
#18243 = CARTESIAN_POINT ( 'NONE',  ( 40.27526882409969744, 92.66518717409400097, 30.44471234641812174 ) ) ;
#18244 = EDGE_CURVE ( 'NONE', #2204, #1699, #17193, .T. ) ;
#18245 = DIRECTION ( 'NONE',  ( 0.000000000000000000, 0.000000000000000000, 1.000000000000000000 ) ) ;
#18246 = VERTEX_POINT ( 'NONE', #13810 ) ;
#18247 = PLANE ( 'NONE',  #16103 ) ;
#18248 = CARTESIAN_POINT ( 'NONE',  ( 11.39584491653312526, 106.7788786240791978, 8.648593811254444930 ) ) ;
#18249 = CARTESIAN_POINT ( 'NONE',  ( 46.59305225739526435, 145.5797705074273267, 36.81289934271958941 ) ) ;
#18250 = CARTESIAN_POINT ( 'NONE',  ( 71.12409474721032154, 120.5409021055102841, -0.3630727742139398528 ) ) ;
#18251 = CARTESIAN_POINT ( 'NONE',  ( 47.43856463449117200, 109.4651871740940123, 35.64915139335016647 ) ) ;
#18252 = CARTESIAN_POINT ( 'NONE',  ( 41.64333658814960870, 68.77977050742731535, 30.00020018409699318 ) ) ;
#18253 = VERTEX_POINT ( 'NONE', #17434 ) ;
#18254 = CARTESIAN_POINT ( 'NONE',  ( 40.27526882409969033, 143.9297705074273210, 30.44471234641811819 ) ) ;
#18255 = CARTESIAN_POINT ( 'NONE',  ( 45.74753988029933538, 97.42977050742730682, 37.97664729208901946 ) ) ;
#18256 = CARTESIAN_POINT ( 'NONE',  ( 41.46631938032478359, 142.3104996726487457, 38.96596240072933170 ) ) ;
#18257 = CARTESIAN_POINT ( 'NONE',  ( 41.46631938032478359, 111.1104996726487428, 29.45539723777780239 ) ) ;
#18258 = CARTESIAN_POINT ( 'NONE',  ( 47.43856463449117200, 64.46518717409398391, 35.64915139335016647 ) ) ;
#18259 = DIRECTION ( 'NONE',  ( 0.000000000000000000, 0.000000000000000000, 1.000000000000000000 ) ) ;
#18260 = CARTESIAN_POINT ( 'NONE',  ( -159.0959885057557983, -158.1938272943107222, 44.11586579668791330 ) ) ;
#18261 = CARTESIAN_POINT ( 'NONE',  ( -141.4692556286852891, -165.9891397928654726, 49.65701158161630957 ) ) ;
#18262 = CARTESIAN_POINT ( 'NONE',  ( -151.4692556286852891, -179.3130981290892407, 39.14238933923362396 ) ) ;
#18263 = DIRECTION ( 'NONE',  ( 0.000000000000000000, 0.000000000000000000, 1.000000000000000000 ) ) ;
#18264 = CARTESIAN_POINT ( 'NONE',  ( 38.96631938032478359, 155.4844580088725934, 31.27175355779120025 ) ) ;
#18265 = CARTESIAN_POINT ( 'NONE',  ( 44.37947211624943833, 137.4797705074273324, 30.00020018409699318 ) ) ;
#18266 = CARTESIAN_POINT ( 'NONE',  ( 77.32109437525961937, 120.4276527761501399, 18.57288864564252506 ) ) ;
#18267 = CARTESIAN_POINT ( 'NONE',  ( 39.42975644700377558, 119.8151871740940067, 31.60846029578754468 ) ) ;
#18268 = LINE ( 'NONE', #16384, #4780 ) ;
#18269 = FACE_OUTER_BOUND ( 'NONE', #21517, .T. ) ;
#18270 = CARTESIAN_POINT ( 'NONE',  ( 47.05648932407426344, 139.9104996726487400, 37.14960608071593384 ) ) ;
#18271 = CARTESIAN_POINT ( 'NONE',  ( 11.38715737009742668, 107.0096734253407362, 2.652989958896663225 ) ) ;
#18272 = EDGE_CURVE ( 'NONE', #21213, #5881, #13636, .T. ) ;
#18273 = CARTESIAN_POINT ( 'NONE',  ( 70.84063976188440392, 115.3547488198113200, -1.153064885589385025 ) ) ;
#18274 = CARTESIAN_POINT ( 'NONE',  ( 148.6725454929228079, -61.68114226949890622, 10.00000000000001599 ) ) ;
#18275 = AXIS2_PLACEMENT_3D ( 'NONE', #3411, #1751, #18824 ) ;
#18276 = CARTESIAN_POINT ( 'NONE',  ( 39.42975644700377558, 96.07977050742731251, 31.60846029578754468 ) ) ;
#18277 =( BOUNDED_CURVE ( )  B_SPLINE_CURVE ( 2, ( #9027, #18946, #7160, #20709, #12317, #3846, #750, #10786, #12431, #13863, #19053, #19157, #13970 ),
 .UNSPECIFIED., .F., .F. ) 
 B_SPLINE_CURVE_WITH_KNOTS ( ( 3, 2, 2, 2, 2, 2, 3 ),
 ( 0.7573529411764705621, 0.7588235294117646745, 0.7617647058823528994, 0.7647058823529411242, 0.7676470588235294601, 0.7705882352941176849, 0.7720588235294117974 ),
 .UNSPECIFIED. ) 
 CURVE ( )  GEOMETRIC_REPRESENTATION_ITEM ( )  RATIONAL_B_SPLINE_CURVE ( ( 0.9755282581475768211, 0.9755282581475768211, 1.000000000000000000, 0.9510565162951535312, 1.000000000000000000, 0.9510565162951535312, 1.000000000000000000, 0.9510565162951535312, 1.000000000000000000, 0.9510565162951535312, 1.000000000000000000, 0.9755282581475768211, 0.9755282581475768211 ) ) 
 REPRESENTATION_ITEM ( '' )  );
#18278 = ORIENTED_EDGE ( 'NONE', *, *, #19879, .T. ) ;
#18279 = PLANE ( 'NONE',  #12940 ) ;
#18280 = VERTEX_POINT ( 'NONE', #4004 ) ;
#18281 = CARTESIAN_POINT ( 'NONE',  ( 43.01140435219951286, 81.53445800887257633, 39.46799094044489209 ) ) ;
#18282 = CARTESIAN_POINT ( 'NONE',  ( 48.01140435219951996, 103.4344580088725678, 32.58608133808903773 ) ) ;
#18283 = CARTESIAN_POINT ( 'NONE',  ( 46.10157429594899270, 136.7604996726487627, 38.46393386101376421 ) ) ;
#18285 = CARTESIAN_POINT ( 'NONE',  ( 67.53959295026429288, 106.1551078129065075, 0.2323293680688409690 ) ) ;
#18284 = CARTESIAN_POINT ( 'NONE',  ( 41.64333658814960870, 92.51518717409399528, 30.00020018409699318 ) ) ;
#18286 = CARTESIAN_POINT ( 'NONE',  ( -157.2955611005346270, -169.7084106276440139, 57.67623309621198047 ) ) ;
#18287 = CARTESIAN_POINT ( 'NONE',  ( -142.0420953463936087, -192.3938272943107393, 49.65701158161630957 ) ) ;
#18289 = DIRECTION ( 'NONE',  ( -1.000000000000000000, 0.000000000000000000, 0.000000000000000000 ) ) ;
#18288 = CARTESIAN_POINT ( 'NONE',  ( -154.5594255724347761, -177.9630981290893033, 59.16757674456785310 ) ) ;
#18290 = CARTESIAN_POINT ( 'NONE',  ( -151.4692556286852891, -126.9891397928655010, 59.65701158161632378 ) ) ;
#18291 = AXIS2_PLACEMENT_3D ( 'NONE', #1424, #1312, #8047 ) ;
#18292 = CARTESIAN_POINT ( 'NONE',  ( 39.92123440845005433, 147.2604996726487343, 29.95742577749336988 ) ) ;
#18293 = CARTESIAN_POINT ( 'NONE',  ( 43.01140435219951286, 77.96049967264873715, 29.21067981925356705 ) ) ;
#18294 = CARTESIAN_POINT ( 'NONE',  ( 38.58424406990786082, 63.11518717409400381, 34.21067981925357060 ) ) ;
#18295 = LINE ( 'NONE', #8274, #13642 ) ;
#18296 = CARTESIAN_POINT ( 'NONE',  ( 61.01612483116806374, 90.79174121657607088, -0.2798613066081144796 ) ) ;
#18297 = CARTESIAN_POINT ( 'NONE',  ( 44.37947211624943833, 149.2151871740940123, 30.00020018409699318 ) ) ;
#18298 = CARTESIAN_POINT ( 'NONE',  ( -151.4692556286852891, -163.1438272943106824, 59.56931450028537967 ) ) ;
#18299 = CARTESIAN_POINT ( 'NONE',  ( -160.8964159109769696, -179.3084106276439798, 46.59394152635518083 ) ) ;
#18300 = ORIENTED_EDGE ( 'NONE', *, *, #17744, .F. ) ;
#18301 = CARTESIAN_POINT ( 'NONE',  ( 41.46631938032478359, 77.18445800887258201, 29.45539723777780239 ) ) ;
#18302 = CARTESIAN_POINT ( 'NONE',  ( -142.0420953463935803, -162.5084106276440536, 46.59394152635518793 ) ) ;
#18303 = CARTESIAN_POINT ( 'NONE',  ( 35.88495058779732716, 86.34054347403214535, 13.57279861601404036 ) ) ;
#18304 = CARTESIAN_POINT ( 'NONE',  ( 45.74753988029933538, 125.0651871740940209, 30.44471234641811819 ) ) ;
#18305 = CARTESIAN_POINT ( 'NONE',  ( 76.02541712503827398, 128.6535784478189726, -7.704039830276845358 ) ) ;
#18306 = VERTEX_POINT ( 'NONE', #3900 ) ;
#18307 = ORIENTED_EDGE ( 'NONE', *, *, #18244, .T. ) ;
#18308 = EDGE_CURVE ( 'NONE', #10912, #9101, #16854, .T. ) ;
#18309 = AXIS2_PLACEMENT_3D ( 'NONE', #17466, #2265, #4034 ) ;
#18310 = CARTESIAN_POINT ( 'NONE',  ( 39.92123440845005433, 147.2344580088725934, 38.46393386101375711 ) ) ;
#18311 = ORIENTED_EDGE ( 'NONE', *, *, #9886, .F. ) ;
#18312 = CARTESIAN_POINT ( 'NONE',  ( 38.96631938032478359, 107.4844580088725792, 31.27175355779120025 ) ) ;
#18313 = CARTESIAN_POINT ( 'NONE',  ( 39.42975644700377558, 159.0797705074273267, 31.60846029578754468 ) ) ;
#18314 = CARTESIAN_POINT ( 'NONE',  ( 46.59305225739526435, 71.17977050742730682, 31.60846029578754468 ) ) ;
#18316 = CARTESIAN_POINT ( 'NONE',  ( 14.82803154953497859, 120.8649872489531987, 9.204245268424362081 ) ) ;
#18315 = CARTESIAN_POINT ( 'NONE',  ( 41.64333658814960870, 125.5151871740939953, 30.00020018409699318 ) ) ;
#18317 = CARTESIAN_POINT ( 'NONE',  ( 38.01140435219951996, 78.86049967264871441, 35.83527830041810347 ) ) ;
#18318 = DIRECTION ( 'NONE',  ( 0.8660254037844390407, -0.000000000000000000, 0.4999999999999994449 ) ) ;
#18319 = CARTESIAN_POINT ( 'NONE',  ( 38.96631938032478359, 144.4104996726487400, 31.27175355779120025 ) ) ;
#18320 = LINE ( 'NONE', #18542, #474 ) ;
#18321 = CARTESIAN_POINT ( 'NONE',  ( 47.43856463449118621, 88.61518717409400381, 34.21067981925357060 ) ) ;
#18322 = ADVANCED_FACE ( 'NONE', ( #478 ), #19109, .F. ) ;
#18323 = DIRECTION ( 'NONE',  ( -0.000000000000000000, -0.000000000000000000, 1.000000000000000000 ) ) ;
#18324 = CARTESIAN_POINT ( 'NONE',  ( 43.01140435219953417, 141.5344580088726048, 39.21067981925356349 ) ) ;
#18325 = STYLED_ITEM ( 'NONE', ( #13018 ), #62 ) ;
#18326 = ORIENTED_EDGE ( 'NONE', *, *, #21604, .F. ) ;
#18327 = CARTESIAN_POINT ( 'NONE',  ( 41.64333658814960870, 62.77977050742732246, 30.00020018409699318 ) ) ;
#18328 = CARTESIAN_POINT ( 'NONE',  ( -145.6429501568359797, -155.9438272943106938, 41.63779006702063867 ) ) ;
#18329 = CARTESIAN_POINT ( 'NONE',  ( 46.60148787037231699, 85.86292235506145687, 7.220022382731924537 ) ) ;
#18330 = CARTESIAN_POINT ( 'NONE',  ( -151.4692556286852891, -187.4084106276440309, 59.56931450028537967 ) ) ;
#18331 = EDGE_LOOP ( 'NONE', ( #20638, #16265, #11060, #6606 ) ) ;
#18332 = CARTESIAN_POINT ( 'NONE',  ( 46.59305225739526435, 157.9151871740940010, 31.60846029578754468 ) ) ;
#18333 = CARTESIAN_POINT ( 'NONE',  ( 138.4260920561042667, 141.9264758756783351, -5.999999999999976019 ) ) ;
#18334 = CARTESIAN_POINT ( 'NONE',  ( 45.74753988029934249, 115.4297705074273068, 37.97664729208901235 ) ) ;
#18335 = CARTESIAN_POINT ( 'NONE',  ( 11.74529739132928619, 133.8467647624810581, -4.446451035385589279 ) ) ;
#18336 = ORIENTED_EDGE ( 'NONE', *, *, #9932, .F. ) ;
#18337 = CARTESIAN_POINT ( 'NONE',  ( 70.05982654948900290, 127.8813624167294023, -8.653178033719973072 ) ) ;
#18338 = ORIENTED_EDGE ( 'NONE', *, *, #15126, .T. ) ;
#18339 = CARTESIAN_POINT ( 'NONE',  ( 38.58424406990786082, 120.3797705074273239, 34.21067981925357060 ) ) ;
#18340 = DIRECTION ( 'NONE',  ( 0.000000000000000000, 1.000000000000000000, 0.000000000000000000 ) ) ;
#18341 = CARTESIAN_POINT ( 'NONE',  ( 40.27526882409969033, 84.82977050742732672, 37.97664729208901946 ) ) ;
#18342 = CARTESIAN_POINT ( 'NONE',  ( 47.43856463449117200, 157.4651871740940123, 35.64915139335016647 ) ) ;
#18343 = CARTESIAN_POINT ( 'NONE',  ( 30.38027039762175718, 151.3010018550503446, 11.44158087452429129 ) ) ;
#18344 = CARTESIAN_POINT ( 'NONE',  ( 39.92123440845005433, 107.3344580088725877, 29.95742577749336988 ) ) ;
#18345 = DIRECTION ( 'NONE',  ( -1.000000000000000000, 0.000000000000000000, -0.000000000000000000 ) ) ;
#18346 = DIRECTION ( 'NONE',  ( 0.9609502660100632809, 0.2767211344570352782, -0.000000000000000000 ) ) ;
#18347 = CARTESIAN_POINT ( 'NONE',  ( -159.5594255724347761, -179.7891397928654840, 43.77915905869157598 ) ) ;
#18348 = CARTESIAN_POINT ( 'NONE',  ( 41.46631938032478359, 90.38445800887258486, 38.96596240072933170 ) ) ;
#18349 = CARTESIAN_POINT ( 'NONE',  ( 43.01140435219951286, 95.03445800887257633, 29.21067981925356705 ) ) ;
#18350 = CARTESIAN_POINT ( 'NONE',  ( 43.01140435219951286, 98.03445800887257633, 29.21067981925356705 ) ) ;
#18351 = CARTESIAN_POINT ( 'NONE',  ( 43.01140435219951286, 92.62977050742732388, 29.55568802177586463 ) ) ;
#18352 = CARTESIAN_POINT ( 'NONE',  ( 61.21858502650649569, 141.5469622553929128, 17.69968404581608823 ) ) ;
#18353 = CARTESIAN_POINT ( 'NONE',  ( -154.3824083646099439, -182.4938272943107336, 40.69124936498395328 ) ) ;
#18354 = CARTESIAN_POINT ( 'NONE',  ( 38.58424406990786082, 84.11518717409400381, 34.21067981925357060 ) ) ;
#18355 = CARTESIAN_POINT ( 'NONE',  ( 39.92123440845005433, 84.26049967264873430, 29.95742577749336988 ) ) ;
#18356 = EDGE_LOOP ( 'NONE', ( #1090, #14121, #7636, #12445 ) ) ;
#18357 = CARTESIAN_POINT ( 'NONE',  ( -141.4692556286852891, -189.9891397928654726, 49.65701158161630957 ) ) ;
#18358 = CARTESIAN_POINT ( 'NONE',  ( -97.23064952102208736, 13.78046159333444720, 4.000000000000021316 ) ) ;
#18359 = CARTESIAN_POINT ( 'NONE',  ( 54.44380493464903736, 94.21656919670213881, 0.9465279732350617703 ) ) ;
#18360 = CARTESIAN_POINT ( 'NONE',  ( 47.43856463449118621, 64.87977050742730967, 34.21067981925357060 ) ) ;
#18361 = ORIENTED_EDGE ( 'NONE', *, *, #5121, .F. ) ;
#18362 = EDGE_CURVE ( 'NONE', #17102, #20293, #18135, .T. ) ;
#18363 = CARTESIAN_POINT ( 'NONE',  ( 38.58424406990786082, 141.3797705074273381, 34.21067981925357060 ) ) ;
#18364 = AXIS2_PLACEMENT_3D ( 'NONE', #7229, #15693, #2358 ) ;
#18365 = CARTESIAN_POINT ( 'NONE',  ( 43.80332655382220963, 151.5373810949689926, 39.21067981925356349 ) ) ;
#18366 = VECTOR ( 'NONE', #7023, 1000.000000000000000 ) ;
#18367 = CARTESIAN_POINT ( 'NONE',  ( 38.01140435219951996, 111.8604996726487570, 35.83527830041810347 ) ) ;
#18368 = CARTESIAN_POINT ( 'NONE',  ( 44.37947211624943833, 67.01518717409399528, 38.42115945441014446 ) ) ;
#18369 = CYLINDRICAL_SURFACE ( 'NONE', #16249, 4.999999999999997335 ) ;
#18370 = CARTESIAN_POINT ( 'NONE',  ( -157.2955611005345986, -163.4438272943107222, 57.67623309621197336 ) ) ;
#18371 = LINE ( 'NONE', #14731, #19206 ) ;
#18372 = CARTESIAN_POINT ( 'NONE',  ( -157.6495955161842062, -182.0130981290893146, 41.15050349809590102 ) ) ;
#18373 = DIRECTION ( 'NONE',  ( 0.000000000000000000, 0.000000000000000000, 1.000000000000000000 ) ) ;
#18374 = LINE ( 'NONE', #6247, #18820 ) ;
#18375 = CARTESIAN_POINT ( 'NONE',  ( 44.55648932407425633, 151.8844580088725991, 29.45539723777780239 ) ) ;
#18376 = B_SPLINE_CURVE_WITH_KNOTS ( 'NONE', 1,
 ( #2052, #8785 ),
 .UNSPECIFIED., .F., .F.,
 ( 2, 2 ),
 ( 0.000000000000000000, 1.000000000000000000 ),
 .UNSPECIFIED. ) ;
#18377 = CARTESIAN_POINT ( 'NONE',  ( 41.64333658814960870, 119.7797705074273296, 30.00020018409699318 ) ) ;
#18378 = CARTESIAN_POINT ( 'NONE',  ( 57.37541587618559191, 88.74458412249896355, 12.85860293144399513 ) ) ;
#18379 = CARTESIAN_POINT ( 'NONE',  ( -9.888205435155610346, 14.72870593739803624, -25.00000000000000000 ) ) ;
#18380 = CARTESIAN_POINT ( 'NONE',  ( 38.58424406990785371, 114.2651871740940095, 35.64915139335015937 ) ) ;
#18381 = LINE ( 'NONE', #3282, #21627 ) ;
#18382 = AXIS2_PLACEMENT_3D ( 'NONE', #275, #20664, #13198 ) ;
#18384 = CARTESIAN_POINT ( 'NONE',  ( 44.55648932407425633, 65.81049967264873146, 29.45539723777780239 ) ) ;
#18383 = AXIS2_PLACEMENT_3D ( 'NONE', #11618, #18346, #9978 ) ;
#18385 = CARTESIAN_POINT ( 'NONE',  ( 41.83190538388809188, 154.0406478741334126, 4.796127949319595629 ) ) ;
#18386 = CARTESIAN_POINT ( 'NONE',  ( 47.24326884731692644, 147.7868190896643341, 4.084992211255583427 ) ) ;
#18387 = CARTESIAN_POINT ( 'NONE',  ( -151.4692556286852891, -196.9891397928655010, 59.65701158161632378 ) ) ;
#18388 = VECTOR ( 'NONE', #4562, 1000.000000000000000 ) ;
#18389 = CARTESIAN_POINT ( 'NONE',  ( 38.58424406990786082, 96.37977050742732388, 34.21067981925357060 ) ) ;
#18390 = EDGE_CURVE ( 'NONE', #10043, #4009, #12475, .T. ) ;
#18391 = VERTEX_POINT ( 'NONE', #906 ) ;
#18392 = CARTESIAN_POINT ( 'NONE',  ( 48.01140435219951996, 145.2844580088725763, 34.21067981925357060 ) ) ;
#18393 = EDGE_LOOP ( 'NONE', ( #5656, #17346 ) ) ;
#18394 = CARTESIAN_POINT ( 'NONE',  ( 38.96631938032478359, 87.08445800887258770, 37.14960608071593384 ) ) ;
#18395 = DIRECTION ( 'NONE',  ( -0.000000000000000000, 1.000000000000000000, -0.000000000000000000 ) ) ;
#18396 = CARTESIAN_POINT ( 'NONE',  ( 38.01140435219952707, 141.7104996726487514, 34.21067981925357060 ) ) ;
#18398 = CARTESIAN_POINT ( 'NONE',  ( 25.43708531585104993, 141.8584285267105827, 4.160929998272084873 ) ) ;
#18397 = CARTESIAN_POINT ( 'NONE',  ( 43.01140435219951286, 95.36518717409400381, 29.55568802177586463 ) ) ;
#18399 = EDGE_CURVE ( 'NONE', #12683, #18667, #14575, .T. ) ;
#18400 = CARTESIAN_POINT ( 'NONE',  ( -143.8425227516148084, -168.3584106276440480, 44.11586579668791330 ) ) ;
#18401 = CARTESIAN_POINT ( 'NONE',  ( -151.4692556286852891, -193.1438272943107393, 59.56931450028537256 ) ) ;
#18403 = CARTESIAN_POINT ( 'NONE',  ( 111.4021762516569964, 137.5714195593754710, 272.0939500981630204 ) ) ;
#18402 = LINE ( 'NONE', #1535, #16072 ) ;
#18404 = LINE ( 'NONE', #8270, #4545 ) ;
#18405 = CARTESIAN_POINT ( 'NONE',  ( -141.4692556286852891, -177.0630981290893260, 49.65701158161630957 ) ) ;
#18406 = CARTESIAN_POINT ( 'NONE',  ( 44.55648932407425633, 79.61049967264874283, 38.96596240072933170 ) ) ;
#18407 = CARTESIAN_POINT ( 'NONE',  ( 41.64333658814960870, 152.7797705074273438, 30.00020018409699318 ) ) ;
#18408 = DIRECTION ( 'NONE',  ( -1.000000000000000000, 0.000000000000000000, 0.000000000000000000 ) ) ;
#18409 = CARTESIAN_POINT ( 'NONE',  ( 74.85601106972485752, 107.3429126181175661, -0.9942341299615756745 ) ) ;
#18410 = CARTESIAN_POINT ( 'NONE',  ( 38.58424406990785371, 141.2651871740939953, 35.64915139335015937 ) ) ;
#18411 = CARTESIAN_POINT ( 'NONE',  ( -154.3824083646099439, -161.4938272943107336, 40.69124936498395328 ) ) ;
#18412 = CARTESIAN_POINT ( 'NONE',  ( -159.0959885057557983, -179.4584106276440707, 44.11586579668791330 ) ) ;
#18413 = ADVANCED_FACE ( 'NONE', ( #14674 ), #14455, .T. ) ;
#18414 = ADVANCED_FACE ( 'NONE', ( #16114 ), #2887, .T. ) ;
#18415 = ORIENTED_EDGE ( 'NONE', *, *, #20304, .T. ) ;
#18416 = LINE ( 'NONE', #16748, #18728 ) ;
#18417 =( BOUNDED_CURVE ( )  B_SPLINE_CURVE ( 2, ( #19925, #11537, #21692, #14945, #6591, #13310, #12079, #12184, #2266, #20684, #20470, #3714, #12291 ),
 .UNSPECIFIED., .F., .F. ) 
 B_SPLINE_CURVE_WITH_KNOTS ( ( 3, 2, 2, 2, 2, 2, 3 ),
 ( 0.08928571428571421831, 0.09285714285714286031, 0.1000000000000000056, 0.1071428571428571369, 0.1142857142857142821, 0.1214285714285714274, 0.1249999999999999584 ),
 .UNSPECIFIED. ) 
 CURVE ( )  GEOMETRIC_REPRESENTATION_ITEM ( )  RATIONAL_B_SPLINE_CURVE ( ( 0.9755282581475768211, 0.9755282581475763770, 1.000000000000000000, 0.9510565162951535312, 1.000000000000000000, 0.9510565162951535312, 1.000000000000000000, 0.9510565162951535312, 1.000000000000000000, 0.9510565162951535312, 1.000000000000000000, 0.9755282581475770431, 0.9755282581475768211 ) ) 
 REPRESENTATION_ITEM ( '' )  );
#18418 = CARTESIAN_POINT ( 'NONE',  ( -142.0420953463936087, -159.6584106276440593, 49.65701158161630957 ) ) ;
#18419 = CARTESIAN_POINT ( 'NONE',  ( 29.98029990418277180, 151.1550010424932111, 23.43402463578956585 ) ) ;
#18420 = CARTESIAN_POINT ( 'NONE',  ( 38.96631938032478359, 134.4844580088725934, 31.27175355779120025 ) ) ;
#18421 = CARTESIAN_POINT ( 'NONE',  ( 43.01140435219951286, 120.8651871740940180, 38.86567161673127657 ) ) ;
#18422 = ORIENTED_EDGE ( 'NONE', *, *, #20748, .T. ) ;
#18423 = ORIENTED_EDGE ( 'NONE', *, *, #15318, .F. ) ;
#18424 = CARTESIAN_POINT ( 'NONE',  ( 147.8787791192428074, -136.9891397928655010, 59.65701158161630957 ) ) ;
#18425 = ORIENTED_EDGE ( 'NONE', *, *, #15368, .F. ) ;
#18426 = CARTESIAN_POINT ( 'NONE',  ( 48.01140435219951996, 109.4344580088725820, 32.58608133808903773 ) ) ;
#18427 = CARTESIAN_POINT ( 'NONE',  ( 44.37947211624943833, 70.27977050742731535, 38.42115945441014446 ) ) ;
#18429 = CARTESIAN_POINT ( 'NONE',  ( 29.72792815944318789, 144.7825833525567134, 3.370790685444458479 ) ) ;
#18428 = CARTESIAN_POINT ( 'NONE',  ( 47.43856463449117200, 130.4651871740939839, 35.64915139335016647 ) ) ;
#18430 = CARTESIAN_POINT ( 'NONE',  ( 46.10157429594899270, 77.66049967264871157, 29.95742577749337343 ) ) ;
#18431 = CARTESIAN_POINT ( 'NONE',  ( 31.47436479266152531, 87.67613096727390598, 14.72005176623422606 ) ) ;
#18432 = DIRECTION ( 'NONE',  ( -0.000000000000000000, -0.000000000000000000, 1.000000000000000000 ) ) ;
#18433 = CYLINDRICAL_SURFACE ( 'NONE', #21712, 10.00000000000003730 ) ;
#18434 = CARTESIAN_POINT ( 'NONE',  ( 45.74753988029933538, 86.06518717409400665, 30.44471234641811819 ) ) ;
#18435 = CARTESIAN_POINT ( 'NONE',  ( 38.26681966641773158, 144.4530603969024014, 32.59926919370181508 ) ) ;
#18436 = FACE_OUTER_BOUND ( 'NONE', #19068, .T. ) ;
#18437 = EDGE_CURVE ( 'NONE', #5574, #4775, #2779, .T. ) ;
#18438 = ORIENTED_EDGE ( 'NONE', *, *, #18752, .T. ) ;
#18439 = CARTESIAN_POINT ( 'NONE',  ( 41.64333658814960870, 63.97977050742731109, 38.42115945441014446 ) ) ;
#18440 = CARTESIAN_POINT ( 'NONE',  ( -148.5561028927606344, -187.2584106276440536, 58.62277379824867296 ) ) ;
#18441 = CARTESIAN_POINT ( 'NONE',  ( 63.43270131736515083, 147.4839633491013728, -3.451138109367889228 ) ) ;
#18442 = CARTESIAN_POINT ( 'NONE',  ( -159.0959885057557983, -179.4584106276440707, 44.11586579668791330 ) ) ;
#18443 = EDGE_LOOP ( 'NONE', ( #12523, #21072, #37, #10162 ) ) ;
#18444 =( REPRESENTATION_RELATIONSHIP ('NONE','NONE', #6933, #3970 ) REPRESENTATION_RELATIONSHIP_WITH_TRANSFORMATION ( #6683 )SHAPE_REPRESENTATION_RELATIONSHIP( ) );
#18445 = CARTESIAN_POINT ( 'NONE',  ( 38.58424406990784661, 153.2651871740940237, 35.64915139335016647 ) ) ;
#18446 = CARTESIAN_POINT ( 'NONE',  ( -149.8854112254399240, -160.6622583705451461, 59.65701158161632378 ) ) ;
#18447 = CARTESIAN_POINT ( 'NONE',  ( 38.58424406990785371, 111.5297705074273296, 35.64915139335015937 ) ) ;
#18448 = CARTESIAN_POINT ( 'NONE',  ( 32.31036143884366396, 152.4250368413922274, -10.51794503956956817 ) ) ;
#18449 = EDGE_LOOP ( 'NONE', ( #7094, #6315, #5077, #12638, #20513, #14394, #16878, #5963, #3035 ) ) ;
#18450 = CARTESIAN_POINT ( 'NONE',  ( 18.86999673272213229, 105.3337293714367604, -5.438779171309367833 ) ) ;
#18451 = VERTEX_POINT ( 'NONE', #4318 ) ;
#18452 = CARTESIAN_POINT ( 'NONE',  ( 43.01140435219951286, 116.6297705074273097, 29.55568802177586463 ) ) ;
#18453 = CARTESIAN_POINT ( 'NONE',  ( 39.92123440845005433, 128.3344580088725877, 29.95742577749336988 ) ) ;
#18454 = CARTESIAN_POINT ( 'NONE',  ( 40.27526882409969033, 156.5651871740939498, 37.97664729208901946 ) ) ;
#18455 = CARTESIAN_POINT ( 'NONE',  ( 77.22348061889915982, 118.7203125366680752, -8.375138532479306619 ) ) ;
#18456 = FILL_AREA_STYLE ('',( #155 ) ) ;
#18457 = CARTESIAN_POINT ( 'NONE',  ( -151.4692556286852891, -196.9891397928655010, 49.65701158161630957 ) ) ;
#18458 = CARTESIAN_POINT ( 'NONE',  ( -141.4692556286852891, -177.8391397928654385, 46.40781461928724383 ) ) ;
#18459 = CARTESIAN_POINT ( 'NONE',  ( 38.96631938032478359, 157.0104996726487343, 37.14960608071593384 ) ) ;
#18460 = PLANE ( 'NONE',  #6545 ) ;
#18461 = CARTESIAN_POINT ( 'NONE',  ( 116.9721770337685740, 133.1239846058259388, -25.00000000000000000 ) ) ;
#18462 = LINE ( 'NONE', #17119, #6771 ) ;
#18463 = CARTESIAN_POINT ( 'NONE',  ( 45.74753988029933538, 91.42977050742732104, 37.97664729208901946 ) ) ;
#18464 = CARTESIAN_POINT ( 'NONE',  ( 62.59245796673033624, 99.61375035622579333, -0.4388640268946644718 ) ) ;
#18465 = CARTESIAN_POINT ( 'NONE',  ( -142.0420953463935803, -171.2438272943107052, 46.59394152635518793 ) ) ;
#18466 = VECTOR ( 'NONE', #9055, 1000.000000000000000 ) ;
#18467 = CARTESIAN_POINT ( 'NONE',  ( 44.37947211624943833, 92.21518717409401233, 30.00020018409699318 ) ) ;
#18468 = CARTESIAN_POINT ( 'NONE',  ( 39.92123440845005433, 85.16049967264873999, 38.46393386101375711 ) ) ;
#18469 = VERTEX_POINT ( 'NONE', #1020 ) ;
#18470 = CARTESIAN_POINT ( 'NONE',  ( 39.92123440845005433, 137.3344580088725593, 29.95742577749336988 ) ) ;
#18471 = CARTESIAN_POINT ( 'NONE',  ( 75.40436159597490473, 130.9804297329818326, 12.22031048084446248 ) ) ;
#18472 = CARTESIAN_POINT ( 'NONE',  ( 14.91610048035210312, 121.0785340954179645, 3.208644154750278865 ) ) ;
#18473 = CARTESIAN_POINT ( 'NONE',  ( 46.59305225739526435, 62.17977050742732104, 31.60846029578754468 ) ) ;
#18474 = ORIENTED_EDGE ( 'NONE', *, *, #5917, .F. ) ;
#18475 = CARTESIAN_POINT ( 'NONE',  ( 46.59305225739526435, 142.5797705074273267, 36.81289934271958941 ) ) ;
#18476 = CARTESIAN_POINT ( 'NONE',  ( 47.43856463449118621, 94.87977050742732388, 34.21067981925357060 ) ) ;
#18477 = CARTESIAN_POINT ( 'NONE',  ( 121.4021762516569964, 137.5714195593754710, -35.00000000000000000 ) ) ;
#18478 = CARTESIAN_POINT ( 'NONE',  ( 44.55648932407425633, 100.6104996726487286, 38.96596240072933170 ) ) ;
#18479 = DIRECTION ( 'NONE',  ( 0.000000000000000000, 0.000000000000000000, 1.000000000000000000 ) ) ;
#18480 = CARTESIAN_POINT ( 'NONE',  ( -81.61981105773979550, 604.5992151483073940, -0.8325491102011938205 ) ) ;
#18481 = CARTESIAN_POINT ( 'NONE',  ( -142.0420953463935803, -165.5438272943107165, 52.72008163687743831 ) ) ;
#18482 = CARTESIAN_POINT ( 'NONE',  ( 76.17254549292280785, -61.68114226949890622, 30.00000000000000000 ) ) ;
#18483 = CARTESIAN_POINT ( 'NONE',  ( -154.5594255724347761, -171.9630981290893033, 59.16757674456785310 ) ) ;
#18484 =( NAMED_UNIT ( * ) SI_UNIT ( $, .STERADIAN. ) SOLID_ANGLE_UNIT ( ) );
#18485 = CARTESIAN_POINT ( 'NONE',  ( 38.01140435219951996, 140.9344580088725820, 35.83527830041810347 ) ) ;
#18486 = CARTESIAN_POINT ( 'NONE',  ( 39.42975644700377558, 123.6797705074273210, 36.81289934271958941 ) ) ;
#18487 = CARTESIAN_POINT ( 'NONE',  ( 61.62447910614003632, 148.7338836329059859, 10.47761036752830144 ) ) ;
#18488 = DIRECTION ( 'NONE',  ( 0.000000000000000000, 1.000000000000000000, 0.000000000000000000 ) ) ;
#18489 = CARTESIAN_POINT ( 'NONE',  ( 43.01140435219951286, 117.8651871740939896, 38.86567161673127657 ) ) ;
#18490 = DIRECTION ( 'NONE',  ( 0.000000000000000000, 0.000000000000000000, 1.000000000000000000 ) ) ;
#18491 = CARTESIAN_POINT ( 'NONE',  ( 42.21948215057684450, 125.1113394311928460, 29.21067981925356705 ) ) ;
#18492 = EDGE_CURVE ( 'NONE', #18531, #4997, #12201, .T. ) ;
#18493 = CARTESIAN_POINT ( 'NONE',  ( 56.91482361236938203, 88.71218622616480332, 0.8673887411229855848 ) ) ;
#18494 = CARTESIAN_POINT ( 'NONE',  ( 62.59245796673033624, 99.61375035622579333, -0.4388640268946644718 ) ) ;
#18495 = CYLINDRICAL_SURFACE ( 'NONE', #20268, 21.90454335994848734 ) ;
#18496 = CARTESIAN_POINT ( 'NONE',  ( 44.37947211624943833, 83.47977050742731819, 30.00020018409699318 ) ) ;
#18497 = EDGE_LOOP ( 'NONE', ( #19044, #1748 ) ) ;
#18498 = VECTOR ( 'NONE', #6370, 1000.000000000000000 ) ;
#18499 = DIRECTION ( 'NONE',  ( -0.000000000000000000, -0.000000000000000000, 1.000000000000000000 ) ) ;
#18500 = ORIENTED_EDGE ( 'NONE', *, *, #15713, .F. ) ;
#18501 = CARTESIAN_POINT ( 'NONE',  ( 47.05648932407426344, 72.98445800887257917, 37.14960608071593384 ) ) ;
#18502 = CARTESIAN_POINT ( 'NONE',  ( 43.01140435219951286, 86.03445800887256212, 29.21067981925356705 ) ) ;
#18503 = CARTESIAN_POINT ( 'NONE',  ( 41.46631938032478359, 141.1104996726487286, 29.45539723777780239 ) ) ;
#18505 = CARTESIAN_POINT ( 'NONE',  ( 26.51748177580332566, 149.8140053266110385, -9.728054792207391444 ) ) ;
#18504 = CARTESIAN_POINT ( 'NONE',  ( 46.59305225739526435, 85.91518717409400097, 31.60846029578754468 ) ) ;
#18506 = CARTESIAN_POINT ( 'NONE',  ( -142.0420953463935803, -159.5084106276440536, 46.59394152635518793 ) ) ;
#18507 = CARTESIAN_POINT ( 'NONE',  ( -159.0959885057557983, -191.1938272943107222, 44.11586579668791330 ) ) ;
#18508 = CARTESIAN_POINT ( 'NONE',  ( 134.6380592378699532, 268.5785371414991687, -19.99999999999997868 ) ) ;
#18509 = DIRECTION ( 'NONE',  ( -0.000000000000000000, -0.000000000000000000, -1.000000000000000000 ) ) ;
#18510 = EDGE_CURVE ( 'NONE', #10554, #19098, #16218, .T. ) ;
#18511 = LINE ( 'NONE', #3421, #12821 ) ;
#18512 = DIRECTION ( 'NONE',  ( -1.000000000000000000, -0.000000000000000000, -0.000000000000000000 ) ) ;
#18513 = CARTESIAN_POINT ( 'NONE',  ( 41.64333658814960870, 155.7797705074273438, 30.00020018409699318 ) ) ;
#18514 = DIRECTION ( 'NONE',  ( -1.140132994654635861E-16, -0.000000000000000000, -1.000000000000000000 ) ) ;
#18515 = EDGE_CURVE ( 'NONE', #1525, #19662, #2371, .T. ) ;
#18516 = CARTESIAN_POINT ( 'NONE',  ( 69.83118287335672392, 141.1824132108841638, 4.838974892866481525 ) ) ;
#18517 = CARTESIAN_POINT ( 'NONE',  ( 40.27526882409969744, 146.6651871740940294, 30.44471234641812174 ) ) ;
#18518 = AXIS2_PLACEMENT_3D ( 'NONE', #1456, #14890, #3219 ) ;
#18519 = CARTESIAN_POINT ( 'NONE',  ( -154.3824083646099439, -164.4938272943107336, 40.69124936498395328 ) ) ;
#18520 = CARTESIAN_POINT ( 'NONE',  ( -148.5561028927606344, -171.0584106276440366, 40.69124936498395328 ) ) ;
#18521 = ORIENTED_EDGE ( 'NONE', *, *, #18525, .T. ) ;
#18522 = CARTESIAN_POINT ( 'NONE',  ( 39.42975644700377558, 63.41518717409400097, 36.81289934271958941 ) ) ;
#18523 = CARTESIAN_POINT ( 'NONE',  ( -160.8964159109769696, -164.0084106276440536, 52.72008163687743121 ) ) ;
#18524 = CARTESIAN_POINT ( 'NONE',  ( 33.94330515458147346, 146.6952251797808628, -4.443226218224292978 ) ) ;
#18525 = EDGE_CURVE ( 'NONE', #3863, #3266, #254, .T. ) ;
#18526 = CARTESIAN_POINT ( 'NONE',  ( 38.01140435219952707, 134.6344580088725422, 32.58608133808903773 ) ) ;
#18527 = CARTESIAN_POINT ( 'NONE',  ( 46.59305225739526435, 127.3151871740940067, 36.81289934271958941 ) ) ;
#18528 = EDGE_LOOP ( 'NONE', ( #11026, #1778, #8287, #1025 ) ) ;
#18529 = VERTEX_POINT ( 'NONE', #11811 ) ;
#18530 = CARTESIAN_POINT ( 'NONE',  ( 43.01140435219951996, 147.5344580088726048, 39.21067981925356349 ) ) ;
#18531 = VERTEX_POINT ( 'NONE', #16767 ) ;
#18532 = CARTESIAN_POINT ( 'NONE',  ( 39.92123440845004723, 98.33445800887258770, 29.95742577749337343 ) ) ;
#18533 = EDGE_CURVE ( 'NONE', #12336, #17794, #5095, .T. ) ;
#18534 = CARTESIAN_POINT ( 'NONE',  ( 45.74753988029933538, 70.42977050742730682, 37.97664729208901946 ) ) ;
#18536 = CARTESIAN_POINT ( 'NONE',  ( 20.72232308940363765, 137.1362251821529696, 16.90007324815861267 ) ) ;
#18535 = CARTESIAN_POINT ( 'NONE',  ( 43.01140435219951286, 126.8651871740940180, 38.86567161673127657 ) ) ;
#18537 = VECTOR ( 'NONE', #8318, 1000.000000000000227 ) ;
#18538 = CARTESIAN_POINT ( 'NONE',  ( 44.55648932407425633, 82.61049967264874283, 38.96596240072933170 ) ) ;
#18539 = CARTESIAN_POINT ( 'NONE',  ( 57.67197451322198276, 240.2871645992281628, -19.99999999999997868 ) ) ;
#18540 = EDGE_CURVE ( 'NONE', #8611, #15790, #18202, .T. ) ;
#18541 = CARTESIAN_POINT ( 'NONE',  ( 38.01140435219952707, 144.8604996726487286, 35.83527830041809636 ) ) ;
#18542 = CARTESIAN_POINT ( 'NONE',  ( 139.9279279298906147, 262.8829071470229906, -5.999999999999976019 ) ) ;
#18543 =( BOUNDED_SURFACE ( )  B_SPLINE_SURFACE ( 1, 2, ( 
 ( #848, #6123, #5912, #12640, #19362, #11301, #4260, #10987, #17698, #18027, #1172, #19573, #2601, #15938, #4159, #8017, #14724, #9340, #21347, #7905, #6237, #16266, #21459, #7583, #12967, #6349, #14284, #14608, #2822, #953, #17802, #16370, #14395, #2934, #21029, #4581, #19689, #2713, #9456, #7698, #21245, #21134, #9670, #1067, #1281, #12852, #6017, #12748, #13075, #11198, #19469, #10889, #17592, #4359, #11089, #4467, #7798, #17911, #9560, #1393, #10217, #13514, #9781, #13407, #6805, #21791, #176, #11857, #3155, #21571, #3379, #8123, #11524, #11409, #9887, #3042, #10105, #6461, #8564, #20138, #16920, #1832, #16812, #19915, #16702, #15278, #18134, #1504, #14935, #4802, #1726, #9997, #20248, #66, #21684, #5139, #13182, #6909, #19803, #1609, #18587, #13299, #16476, #18254, #11743, #16585, #4693, #14825, #5034, #6580, #6698, #8342, #18475, #8234, #20035, #8459, #15165, #3494, #4920, #11633, #18363, #3267, #15052, #20779, #7124, #8779, #2153, #13935, #8992, #17455, #20353, #15700, #10324, #15593, #11965, #715, #20675, #3597, #5671, #12394, #10646, #606, #7235, #14045, #9104, #17026, #1937, #4023, #19129, #8669, #5558, #10751, #498, #15803, #2365, #18800, #15393, #19019, #288, #5352, #5247, #3702, #18696, #3919, #7019, #13615, #12282, #13723, #20460, #17349, #12069, #10539, #10430, #17135, #2050, #15494, #396, #2257, #3813, #13831, #20569, #5453, #12172, #18907, #17238, #8886, #19442, #9538, #926, #20887, #14254, #21216, #19335, #19663, #12504, #7774, #2575, #9424, #4335, #16130, #19231, #7556, #14472, #2796, #16235, #17995, #1039, #4555, #10864, #9211, #14580, #7671, #9314, #17776, #6096, #1146, #11275, #14151, #7881, #4130, #12826, #15908, #819, #20998, #21324, #4440, #19545, #5883, #17563, #7447, #2910, #9643, #12614, #6209, #11172, #12939, #17883, #16345, #2469, #5775, #4235, #10962, #17672, #16015, #14369, #21109, #5991, #12719, #11061, #2681, #1700, #8429, #14909, #21659, #1364, #11611, #9754, #5007, #6549, #10078, #18339, #13049, #15138, #6435, #3016, #6672, #8095, #14802, #21433, #13159, #6322, #20116, #21543, #11830, #8317, #20220, #13488, #11717, #19888, #20007, #10192, #4776, #11496, #18225, #3129, #18452, #13272, #41, #3352, #9859, #6781, #16560, #5113, #1252, #4891, #7989, #1476, #8208, #3241, #15025, #9972, #16675, #6881, #2125, #2021, #3784, #7098, #10513, #13588, #16998, #13907, #12258, #18991, #5642, #3893, #14018, #20326, #18668, #574, #8752, #15469, #12143, #10616, #17323, #12364, #1808, #7318, #5224, #16893, #3571, #1906, #8642, #15364, #256, #6992, #20432, #5326, #20540, #9031, #15742, #324, #20712, #7272, #13974, #15628, #647, #3637, #5595, #7382, #11999, #12322, #8923, #8710, #15528, #2291, #12105, #19057, #18732, #3959, #10682, #433, #7164, #15429, #20605, #1975, #17387, #8818, #14084, #5488, #10362, #20388, #6948, #2192, #17063, #13654, #5285, #7055, #13760, #20500, #5389, #18837, #13867, #12215, #3743, #10472, #18949, #17173, #2086, #3850, #10576, #533, #17277, #18697, #8566, #13616, #5140, #20354, #4804, #1505, #8235, #17028, #5249, #16587, #11858, #3600, #6807, #11525, #10325, #9998, #6581, #10219, #14937, #3268, #18255, #1611, #9888, #16921, #20036, #3157, #18589, #1938, #4923, #6910, #8343, #1727, #15054, #21792, #6700, #5035, #11744, #18476, #16813, #3380, #8461, #15166, #69, #13515, #821, #3703, #10649, #717, #13936, #8780, #5454, #12397, #17240, #398, #7127, #2367, #499, #607, #17351, #13832, #12173, #2154, #20676, #8993, #15701, #3018, #16237, #16453, #21111, #9427, #6324, #21218, #12828, #12942, #11279, #9645, #14256, #21001, #7991, #19547, #17997, #17885, #2912, #14696, #5885, #5115, #13490, #13274, #19890, #14804, #10299, #11498, #20010, #3469, #11832, #15253, #152, #18229, #3131, #13591, #9861, #8210, #4894, #11613, #18341, #20118, #15027, #17212, #7425, #18776, #2338, #20863, #7208, #18995, #13806, #10619, #17108, #5645, #17327, #10729, #8967, #20544, #259, #10839, #577, #20754, #19104, #2127, #12479, #2656, #7646, #19639, #6184, #14558, #16108, #7531, #19750, #9399, #1124, #14233, #12804, #901, #12915, #17754, #21300, #797, #5861, #16213, #21409, #11251, #4531, #7962, #17972, #19313, #9515, #17647, #2881, #4644, #20973, #17536, #2554, #9291, #14669, #4314, #15992, #9620, #7753, #15884, #2446, #1016, #4418, #12695, #14345, #16319, #9186, #4211, #6297, #14451, #17861, #12591, #21087, #21190, #5968, #19417, #11038, #6078, #19525, #11148, #7857, #2775, #16427, #21522, #14996, #15, #4865, #18314, #4981, #11692, #9836, #13562, #18534, #18427, #13463, #21738, #2989, #4748, #16536, #11803, #11362, #8403, #3325, #1562, #18083, #1452, #21632, #10166, #6523, #19861, #1339, #16760, #6646, #20196, #1781, #10054, #20092, #5089, #9730, #8073, #3441, #13244, #3214, #15228, #19980, #15112, #11468, #9947, #20298, #14886, #11586, #1671, #8185, #16650, #6755, #16867, #13355, #8515, #126, #6855, #14779, #6411, #13134, #18197, #3104, #3545, #8725, #344, #12015, #2208, #17187, #20728, #7293, #7073, #5616, #13672, #17404, #5196, #2099, #13992, #20515, #18643, #18749, #18965, #17080, #2309, #10270, #12234 ),
 ( #8939, #16973, #15336, #3868, #9048, #12339, #549, #15757, #15645, #6966, #10591, #20405, #19074, #14100, #1883, #11913, #5303, #3652, #662, #13776, #10380, #3975, #8837, #8617, #228, #12119, #13882, #5402, #1994, #10700, #7399, #15443, #18852, #3760, #17296, #10487, #15543, #448, #7178, #20621, #7933, #12885, #19389, #12669, #11120, #5939, #4078, #9160, #2629, #9484, #14315, #11013, #14425, #21160, #19287, #1198, #6150, #6049, #1095, #9369, #12451, #14206, #4186, #21272, #20836, #17835, #12775, #17724, #5727, #10914, #9264, #19606, #15964, #7506, #10808, #4388, #16074, #7829, #11222, #19496, #7723, #14531, #19179, #17511, #4499, #876, #7613, #2745, #17620, #985, #16183, #17941, #2847, #9591, #16292, #2420, #2528, #15859, #772, #20945, #5827, #12560, #21601, #9809, #2959, #6490, #4718, #16729, #3296, #11659, #13210, #4609, #10135, #19947, #20064, #11330, #9913, #19828, #10024, #14855, #18396, #19718, #9698, #13328, #18503, #8372, #1639, #5061, #15082, #16398, #6612, #8044, #19037, #1752, #18051, #14637, #14749, #21490, #11774, #1421, #6376, #6727, #4832, #12997, #21378, #11555, #1530, #16504, #11438, #13433, #16839, #1309, #20171, #18283, #14962, #13105, #3412, #3185, #6264, #18163, #3071, #8150, #16620, #8262, #4951, #21709, #13537, #18613, #12093, #18939, #1965, #15419, #2076, #8806, #6937, #10673, #15617, #15518, #10566, #18826, #99, #1858, #13643, #8914, #8487, #5479, #421, #20488, #15196, #20378, #18719, #7262, #3626, #16942, #20272, #13856, #5378, #17266, #20703, #7153, #17162, #2178, #6830, #5163, #525, #10350, #314, #12311, #17053, #12204, #8588, #7043, #17376, #11989, #20593, #3839, #5274, #11885, #13963, #5586, #19047, #3731, #3518, #15307, #8698, #3946, #10244, #199, #13749, #10461, #2281, #14181, #12533, #1070, #19260, #10780, #7372, #7700, #21031, #11093, #14506, #16045, #10990, #4363, #15732, #9021, #17805, #4162, #9242, #6126, #10891, #21136, #2396, #15941, #11200, #5802, #17594, #14398, #20918, #2500, #6020, #9457, #851, #21248, #16158, #2716, #7586, #17700, #7800, #12643, #17486, #957, #14287, #5914, #12424, #19364, #4262, #12856, #12751, #19471, #2605, #14073, #19578, #9343, #4470, #20811, #637, #7479, #5701, #19151, #4052, #9133, #15833, #744, #21794, #11637, #13302, #8346, #14939, #19695, #9890, #11303, #20040, #5037, #14613, #17913, #18030, #2936, #15057, #4695, #9673, #10001, #8125, #16268, #2824, #3047, #4807, #13077, #8021, #18367, #20144, #4583, #4926, #9784, #18257, #7910, #1614, #16480, #3269, #16705, #9563, #6703, #1396, #14828, #8237, #18138, #1174, #6240, #21573, #6584, #11412, #6464, #13410, #3160, #21351, #12969, #21686, #16373, #13185, #1286, #14726, #21462, #19806, #6353, #19918, #11529, #16590, #1508, #13912, #5752, #20546, #2448, #11746, #2236, #14126, #5534, #3382, #18881, #4002, #2129, #9188, #16815, #12367, #7212, #14022, #8970, #20756, #2026, #12149, #19106, #7427, #20865, #799, #5647, #15886, #15473, #13808, #19209, #12262, #20651, #579, #10731, #12482, #7533, #18478, #4106, #8756, #17432, #5429, #3790, #10519, #10842, #9077, #2340, #17214, #373, #10108, #14235, #20975, #8864, #17538, #15784, #7103, #690, #15572, #476, #18997, #3897, #10621, #17329, #15675, #7322, #19527, #18087, #16111, #13029, #9293, #6301, #21412, #4420, #11150, #5970, #16216, #14348, #9623, #17864, #14672, #1126, #17649, #4213, #14782, #12917, #2556, #19753, #4647, #2885, #11366, #21302, #2992, #1343, #15994, #903, #9733, #16430, #7649, #6186, #8076, #7860, #5863, #12594, #11040, #21089, #11253, #12697, #19419, #19315, #17756, #10942, #17974, #4316, #7755, #2658, #9402, #1018, #14453, #2777, #7965, #21192, #6080, #12806, #19641, #9517, #14560, #4533, #16322, #1231, #1677, #11695, #8406, #4752, #21636, #6758, #16870, #1785, #10274, #15115, #18646, #3107, #1455, #6859, #15001, #16653, #10057, #18, #8518, #3548, #6414, #15231, #18200, #13467, #8188, #14889, #6527, #13565, #18538, #20199, #13248, #11471, #21525, #16976, #1886, #19984, #130, #3446, #20302, #11806, #8621, #9839, #5200, #13137, #16539, #10170, #5093, #4868, #13358, #11917, #9950, #19866, #11589, #18317, #3218, #20095, #4985, #1566, #16765, #8293, #21742, #18430, #6649, #3328, #5306, #13675, #2423, #552, #12018, #665, #7402, #12342, #2312, #8942, #9051, #10811, #18753, #3655, #5730, #15761, #10383, #15649, #14103, #17299, #17514, #20839, #20518, #17083, #20731, #1998, #7077, #6970, #5405, #20410, #5619, #8729, #4081, #7297, #12454, #19183, #19077, #15446, #12238, #15339, #347, #18855, #10491, #13779, #3978, #5508, #232, #17407, #18968, #12123, #3763, #17190, #2102, #8840, #15547, #451, #10704, #3871, #7182, #13887, #13996, #2212, #20624, #10594, #15862, #17946, #11016, #16078, #13001, #17727, #6153, #9267, #989, #18057, #12672, #2632, #14534, #5942, #9373, #21275, #16296, #7726, #6270, #1203, #2852, #19392, #17838, #9595, #19499, #17624, #7832, #14428, #4289, #19290, #21163, #21061, #11226, #19609, #12888, #6052, #20948, #4614, #12778, #4503, #5831, #4391, #14319, #7937, #11123, #14641, #14209, #4189, #21383, #19722, #11335, #9163, #775, #7510, #10917 ) ),
 .UNSPECIFIED., .F., .F., .T. ) 
 B_SPLINE_SURFACE_WITH_KNOTS ( ( 2, 2 ),
 ( 3, 2, 2, 2, 2, 2, 2, 2, 2, 2, 2, 2, 2, 2, 2, 2, 2, 2, 2, 2, 2, 2, 2, 2, 2, 2, 2, 2, 2, 2, 2, 2, 2, 2, 2, 2, 2, 2, 2, 2, 2, 2, 2, 2, 2, 2, 2, 2, 2, 2, 2, 2, 2, 2, 2, 2, 2, 2, 2, 2, 2, 2, 2, 2, 2, 2, 2, 2, 2, 2, 2, 2, 2, 2, 2, 2, 2, 2, 2, 2, 2, 2, 2, 2, 2, 2, 2, 2, 2, 2, 2, 2, 2, 2, 2, 2, 2, 2, 2, 2, 2, 2, 2, 2, 2, 2, 2, 2, 2, 2, 2, 2, 2, 2, 2, 2, 2, 2, 2, 2, 2, 2, 2, 2, 2, 2, 2, 2, 2, 2, 2, 2, 2, 2, 2, 2, 2, 2, 2, 2, 2, 2, 2, 2, 2, 2, 2, 2, 2, 2, 2, 2, 2, 2, 2, 2, 2, 2, 2, 2, 2, 2, 2, 2, 2, 2, 2, 2, 2, 2, 2, 2, 2, 2, 2, 2, 2, 2, 2, 2, 2, 2, 2, 2, 2, 2, 2, 2, 2, 2, 2, 2, 2, 2, 2, 2, 2, 2, 2, 2, 2, 2, 2, 2, 2, 2, 2, 2, 2, 2, 2, 2, 2, 2, 2, 2, 2, 2, 2, 2, 2, 2, 2, 2, 2, 2, 2, 2, 2, 2, 2, 2, 2, 2, 2, 2, 2, 2, 2, 2, 2, 2, 2, 2, 2, 2, 2, 2, 2, 2, 2, 2, 2, 2, 2, 2, 2, 2, 2, 2, 2, 2, 2, 2, 2, 2, 2, 2, 2, 2, 2, 2, 2, 2, 2, 2, 2, 2, 2, 2, 2, 2, 2, 2, 2, 2, 2, 2, 2, 2, 2, 2, 2, 2, 2, 2, 2, 2, 2, 2, 2, 2, 2, 2, 2, 2, 2, 2, 2, 2, 2, 2, 2, 2, 2, 2, 2, 2, 2, 2, 2, 2, 2, 2, 2, 2, 2, 2, 2, 2, 2, 2, 2, 2, 3 ),
 ( 0.000000000000000000, 1.000000000000000000 ),
 ( 0.000000000000000000, 0.002941176470588235253, 0.005882352941176470507, 0.008823529411764705760, 0.01176470588235294101, 0.01470588235294117627, 0.01764705882352941152, 0.02058823529411764677, 0.02352941176470588203, 0.02647058823529411728, 0.02941176470588235253, 0.03235294117647059126, 0.03529411764705882304, 0.03823529411764706176, 0.04117647058823529355, 0.04411764705882353227, 0.04705882352941176405, 0.05000000000000000278, 0.05294117647058823456, 0.05588235294117647328, 0.05882352941176470507, 0.06176470588235294379, 0.06470588235294118251, 0.06764705882352940736, 0.07058823529411764608, 0.07352941176470588480, 0.07647058823529412352, 0.07941176470588234837, 0.08235294117647058709, 0.08529411764705882582, 0.08823529411764706454, 0.09117647058823528938, 0.09411764705882352811, 0.09705882352941176683, 0.1000000000000000056, 0.1029411764705882304, 0.1058823529411764691, 0.1088235294117647078, 0.1117647058823529466, 0.1147058823529411714, 0.1176470588235294101, 0.1205882352941176489, 0.1235294117647058876, 0.1264705882352941124, 0.1294117647058823650, 0.1323529411764705899, 0.1352941176470588147, 0.1382352941176470673, 0.1411764705882352922, 0.1441176470588235170, 0.1470588235294117696, 0.1499999999999999944, 0.1529411764705882470, 0.1558823529411764719, 0.1588235294117646967, 0.1617647058823529493, 0.1647058823529411742, 0.1676470588235293990, 0.1705882352941176516, 0.1735294117647058765, 0.1764705882352941291, 0.1794117647058823539, 0.1823529411764705788, 0.1852941176470588314, 0.1882352941176470562, 0.1911764705882352811, 0.1941176470588235337, 0.1970588235294117585, 0.2000000000000000111, 0.2029411764705882359, 0.2058823529411764608, 0.2088235294117647134, 0.2117647058823529382, 0.2147058823529411631, 0.2176470588235294157, 0.2205882352941176405, 0.2235294117647058931, 0.2264705882352941180, 0.2294117647058823428, 0.2323529411764705954, 0.2352941176470588203, 0.2382352941176470451, 0.2411764705882352977, 0.2441176470588235226, 0.2470588235294117752, 0.2500000000000000000, 0.2529411764705882248, 0.2558823529411764497, 0.2588235294117647300, 0.2617647058823529549, 0.2647058823529411797, 0.2676470588235294046, 0.2705882352941176294, 0.2735294117647059098, 0.2764705882352941346, 0.2794117647058823595, 0.2823529411764705843, 0.2852941176470588092, 0.2882352941176470340, 0.2911764705882353144, 0.2941176470588235392, 0.2970588235294117641, 0.2999999999999999889, 0.3029411764705882137, 0.3058823529411764941, 0.3088235294117647189, 0.3117647058823529438, 0.3147058823529411686, 0.3176470588235293935, 0.3205882352941176738, 0.3235294117647058987, 0.3264705882352941235, 0.3294117647058823484, 0.3323529411764705732, 0.3352941176470587981, 0.3382352941176470784, 0.3411764705882353033, 0.3441176470588235281, 0.3470588235294117530, 0.3499999999999999778, 0.3529411764705882582, 0.3558823529411764830, 0.3588235294117647078, 0.3617647058823529327, 0.3647058823529411575, 0.3676470588235294379, 0.3705882352941176627, 0.3735294117647058876, 0.3764705882352941124, 0.3794117647058823373, 0.3823529411764705621, 0.3852941176470588425, 0.3882352941176470673, 0.3911764705882352922, 0.3941176470588235170, 0.3970588235294117418, 0.4000000000000000222, 0.4029411764705882470, 0.4058823529411764719, 0.4088235294117646967, 0.4117647058823529216, 0.4147058823529412019, 0.4176470588235294268, 0.4205882352941176516, 0.4235294117647058765, 0.4264705882352941013, 0.4294117647058823262, 0.4323529411764706065, 0.4352941176470588314, 0.4382352941176470562, 0.4411764705882352811, 0.4441176470588235059, 0.4470588235294117863, 0.4500000000000000111, 0.4529411764705882359, 0.4558823529411764608, 0.4588235294117646856, 0.4617647058823529660, 0.4647058823529411908, 0.4676470588235294157, 0.4705882352941176405, 0.4735294117647058654, 0.4764705882352940902, 0.4794117647058823706, 0.4823529411764705954, 0.4852941176470588203, 0.4882352941176470451, 0.4911764705882352700, 0.4941176470588235503, 0.4970588235294117752, 0.5000000000000000000, 0.5029411764705882248, 0.5058823529411764497, 0.5088235294117646745, 0.5117647058823528994, 0.5147058823529411242, 0.5176470588235294601, 0.5205882352941176849, 0.5235294117647059098, 0.5264705882352941346, 0.5294117647058823595, 0.5323529411764705843, 0.5352941176470588092, 0.5382352941176470340, 0.5411764705882352589, 0.5441176470588234837, 0.5470588235294118196, 0.5500000000000000444, 0.5529411764705882693, 0.5558823529411764941, 0.5588235294117647189, 0.5617647058823529438, 0.5647058823529411686, 0.5676470588235293935, 0.5705882352941176183, 0.5735294117647058432, 0.5764705882352940680, 0.5794117647058824039, 0.5823529411764706287, 0.5852941176470588536, 0.5882352941176470784, 0.5911764705882353033, 0.5941176470588235281, 0.5970588235294117530, 0.5999999999999999778, 0.6029411764705882026, 0.6058823529411764275, 0.6088235294117646523, 0.6117647058823529882, 0.6147058823529412130, 0.6176470588235294379, 0.6205882352941176627, 0.6235294117647058876, 0.6264705882352941124, 0.6294117647058823373, 0.6323529411764705621, 0.6352941176470587870, 0.6382352941176470118, 0.6411764705882353477, 0.6441176470588235725, 0.6470588235294117974, 0.6500000000000000222, 0.6529411764705882470, 0.6558823529411764719, 0.6588235294117646967, 0.6617647058823529216, 0.6647058823529411464, 0.6676470588235293713, 0.6705882352941175961, 0.6735294117647059320, 0.6764705882352941568, 0.6794117647058823817, 0.6823529411764706065, 0.6852941176470588314, 0.6882352941176470562, 0.6911764705882352811, 0.6941176470588235059, 0.6970588235294117307, 0.6999999999999999556, 0.7029411764705881804, 0.7058823529411765163, 0.7088235294117647411, 0.7117647058823529660, 0.7147058823529411908, 0.7176470588235294157, 0.7205882352941176405, 0.7235294117647058654, 0.7264705882352940902, 0.7294117647058823151, 0.7323529411764705399, 0.7352941176470588758, 0.7382352941176471006, 0.7411764705882353255, 0.7441176470588235503, 0.7470588235294117752, 0.7500000000000000000, 0.7529411764705882248, 0.7558823529411764497, 0.7588235294117646745, 0.7617647058823528994, 0.7647058823529411242, 0.7676470588235294601, 0.7705882352941176849, 0.7735294117647059098, 0.7764705882352941346, 0.7794117647058823595, 0.7823529411764705843, 0.7852941176470588092, 0.7882352941176470340, 0.7911764705882352589, 0.7941176470588234837, 0.7970588235294118196, 0.8000000000000000444, 0.8029411764705882693, 0.8058823529411764941, 0.8088235294117647189, 0.8117647058823529438, 0.8147058823529411686, 0.8176470588235293935, 0.8205882352941176183, 0.8235294117647058432, 0.8264705882352940680, 0.8294117647058824039, 0.8323529411764706287, 0.8352941176470588536, 0.8382352941176470784, 0.8411764705882353033, 0.8441176470588235281, 0.8470588235294117530, 0.8499999999999999778, 0.8529411764705882026, 0.8558823529411764275, 0.8588235294117646523, 0.8617647058823529882, 0.8647058823529412130, 0.8676470588235294379, 0.8705882352941176627, 0.8735294117647058876, 0.8764705882352941124, 0.8794117647058823373, 0.8823529411764705621, 0.8852941176470587870, 0.8882352941176470118, 0.8911764705882353477, 0.8941176470588235725, 0.8970588235294117974, 0.9000000000000000222, 0.9029411764705882470, 0.9058823529411764719, 0.9088235294117646967, 0.9117647058823529216, 0.9147058823529411464, 0.9176470588235293713, 0.9205882352941175961, 0.9235294117647059320, 0.9264705882352941568, 0.9294117647058823817, 0.9323529411764706065, 0.9352941176470588314, 0.9382352941176470562, 0.9411764705882352811, 0.9441176470588235059, 0.9470588235294117307, 0.9499999999999999556, 0.9529411764705881804, 0.9558823529411765163, 0.9588235294117647411, 0.9617647058823529660, 0.9647058823529411908, 0.9676470588235294157, 0.9705882352941176405, 0.9735294117647058654, 0.9764705882352940902, 0.9794117647058823151, 0.9803958342062289999 ),
 .UNSPECIFIED. ) 
 GEOMETRIC_REPRESENTATION_ITEM ( )  RATIONAL_B_SPLINE_SURFACE ( (
 ( 1.000000000000000000, 0.9510565162951535312, 1.000000000000000000, 0.9510565162951535312, 1.000000000000000000, 0.9510565162951535312, 1.000000000000000000, 0.9510565162951535312, 1.000000000000000000, 0.9510565162951535312, 1.000000000000000000, 0.9510565162951535312, 1.000000000000000000, 0.9510565162951535312, 1.000000000000000000, 0.9510565162951535312, 1.000000000000000000, 0.9510565162951535312, 1.000000000000000000, 0.9510565162951535312, 1.000000000000000000, 0.9510565162951535312, 1.000000000000000000, 0.9510565162951535312, 1.000000000000000000, 0.9510565162951535312, 1.000000000000000000, 0.9510565162951535312, 1.000000000000000000, 0.9510565162951535312, 1.000000000000000000, 0.9510565162951535312, 1.000000000000000000, 0.9510565162951535312, 1.000000000000000000, 0.9510565162951535312, 1.000000000000000000, 0.9510565162951535312, 1.000000000000000000, 0.9510565162951535312, 1.000000000000000000, 0.9510565162951535312, 1.000000000000000000, 0.9510565162951535312, 1.000000000000000000, 0.9510565162951535312, 1.000000000000000000, 0.9510565162951535312, 1.000000000000000000, 0.9510565162951535312, 1.000000000000000000, 0.9510565162951535312, 1.000000000000000000, 0.9510565162951535312, 1.000000000000000000, 0.9510565162951535312, 1.000000000000000000, 0.9510565162951535312, 1.000000000000000000, 0.9510565162951535312, 1.000000000000000000, 0.9510565162951535312, 1.000000000000000000, 0.9510565162951535312, 1.000000000000000000, 0.9510565162951535312, 1.000000000000000000, 0.9510565162951535312, 1.000000000000000000, 0.9510565162951535312, 1.000000000000000000, 0.9510565162951535312, 1.000000000000000000, 0.9510565162951535312, 1.000000000000000000, 0.9510565162951535312, 1.000000000000000000, 0.9510565162951535312, 1.000000000000000000, 0.9510565162951535312, 1.000000000000000000, 0.9510565162951535312, 1.000000000000000000, 0.9510565162951535312, 1.000000000000000000, 0.9510565162951535312, 1.000000000000000000, 0.9510565162951535312, 1.000000000000000000, 0.9510565162951535312, 1.000000000000000000, 0.9510565162951535312, 1.000000000000000000, 0.9510565162951535312, 1.000000000000000000, 0.9510565162951535312, 1.000000000000000000, 0.9510565162951535312, 1.000000000000000000, 0.9510565162951535312, 1.000000000000000000, 0.9510565162951535312, 1.000000000000000000, 0.9510565162951535312, 1.000000000000000000, 0.9510565162951535312, 1.000000000000000000, 0.9510565162951535312, 1.000000000000000000, 0.9510565162951535312, 1.000000000000000000, 0.9510565162951535312, 1.000000000000000000, 0.9510565162951535312, 1.000000000000000000, 0.9510565162951535312, 1.000000000000000000, 0.9510565162951535312, 1.000000000000000000, 0.9510565162951535312, 1.000000000000000000, 0.9510565162951535312, 1.000000000000000000, 0.9510565162951535312, 1.000000000000000000, 0.9510565162951535312, 1.000000000000000000, 0.9510565162951535312, 1.000000000000000000, 0.9510565162951535312, 1.000000000000000000, 0.9510565162951535312, 1.000000000000000000, 0.9510565162951535312, 1.000000000000000000, 0.9510565162951535312, 1.000000000000000000, 0.9510565162951535312, 1.000000000000000000, 0.9510565162951535312, 1.000000000000000000, 0.9510565162951535312, 1.000000000000000000, 0.9510565162951535312, 1.000000000000000000, 0.9510565162951535312, 1.000000000000000000, 0.9510565162951535312, 1.000000000000000000, 0.9510565162951535312, 1.000000000000000000, 0.9510565162951535312, 1.000000000000000000, 0.9510565162951535312, 1.000000000000000000, 0.9510565162951535312, 1.000000000000000000, 0.9510565162951535312, 1.000000000000000000, 0.9510565162951535312, 1.000000000000000000, 0.9510565162951535312, 1.000000000000000000, 0.9510565162951535312, 1.000000000000000000, 0.9510565162951535312, 1.000000000000000000, 0.9510565162951535312, 1.000000000000000000, 0.9510565162951535312, 1.000000000000000000, 0.9510565162951535312, 1.000000000000000000, 0.9510565162951535312, 1.000000000000000000, 0.9510565162951535312, 1.000000000000000000, 0.9510565162951535312, 1.000000000000000000, 0.9510565162951535312, 1.000000000000000000, 0.9510565162951535312, 1.000000000000000000, 0.9510565162951535312, 1.000000000000000000, 0.9510565162951535312, 1.000000000000000000, 0.9510565162951535312, 1.000000000000000000, 0.9510565162951535312, 1.000000000000000000, 0.9510565162951535312, 1.000000000000000000, 0.9510565162951535312, 1.000000000000000000, 0.9510565162951535312, 1.000000000000000000, 0.9510565162951535312, 1.000000000000000000, 0.9510565162951535312, 1.000000000000000000, 0.9510565162951535312, 1.000000000000000000, 0.9510565162951535312, 1.000000000000000000, 0.9510565162951535312, 1.000000000000000000, 0.9510565162951535312, 1.000000000000000000, 0.9510565162951535312, 1.000000000000000000, 0.9510565162951535312, 1.000000000000000000, 0.9510565162951535312, 1.000000000000000000, 0.9510565162951535312, 1.000000000000000000, 0.9510565162951535312, 1.000000000000000000, 0.9510565162951535312, 1.000000000000000000, 0.9510565162951535312, 1.000000000000000000, 0.9510565162951535312, 1.000000000000000000, 0.9510565162951535312, 1.000000000000000000, 0.9510565162951535312, 1.000000000000000000, 0.9510565162951535312, 1.000000000000000000, 0.9510565162951535312, 1.000000000000000000, 0.9510565162951535312, 1.000000000000000000, 0.9510565162951535312, 1.000000000000000000, 0.9510565162951535312, 1.000000000000000000, 0.9510565162951535312, 1.000000000000000000, 0.9510565162951535312, 1.000000000000000000, 0.9510565162951535312, 1.000000000000000000, 0.9510565162951535312, 1.000000000000000000, 0.9510565162951535312, 1.000000000000000000, 0.9510565162951535312, 1.000000000000000000, 0.9510565162951535312, 1.000000000000000000, 0.9510565162951535312, 1.000000000000000000, 0.9510565162951535312, 1.000000000000000000, 0.9510565162951535312, 1.000000000000000000, 0.9510565162951535312, 1.000000000000000000, 0.9510565162951535312, 1.000000000000000000, 0.9510565162951535312, 1.000000000000000000, 0.9510565162951535312, 1.000000000000000000, 0.9510565162951535312, 1.000000000000000000, 0.9510565162951535312, 1.000000000000000000, 0.9510565162951535312, 1.000000000000000000, 0.9510565162951535312, 1.000000000000000000, 0.9510565162951535312, 1.000000000000000000, 0.9510565162951535312, 1.000000000000000000, 0.9510565162951535312, 1.000000000000000000, 0.9510565162951535312, 1.000000000000000000, 0.9510565162951535312, 1.000000000000000000, 0.9510565162951535312, 1.000000000000000000, 0.9510565162951535312, 1.000000000000000000, 0.9510565162951535312, 1.000000000000000000, 0.9510565162951535312, 1.000000000000000000, 0.9510565162951535312, 1.000000000000000000, 0.9510565162951535312, 1.000000000000000000, 0.9510565162951535312, 1.000000000000000000, 0.9510565162951535312, 1.000000000000000000, 0.9510565162951535312, 1.000000000000000000, 0.9510565162951535312, 1.000000000000000000, 0.9510565162951535312, 1.000000000000000000, 0.9510565162951535312, 1.000000000000000000, 0.9510565162951535312, 1.000000000000000000, 0.9510565162951535312, 1.000000000000000000, 0.9510565162951535312, 1.000000000000000000, 0.9510565162951535312, 1.000000000000000000, 0.9510565162951535312, 1.000000000000000000, 0.9510565162951535312, 1.000000000000000000, 0.9510565162951535312, 1.000000000000000000, 0.9510565162951535312, 1.000000000000000000, 0.9510565162951535312, 1.000000000000000000, 0.9510565162951535312, 1.000000000000000000, 0.9510565162951535312, 1.000000000000000000, 0.9510565162951535312, 1.000000000000000000, 0.9510565162951535312, 1.000000000000000000, 0.9510565162951535312, 1.000000000000000000, 0.9510565162951535312, 1.000000000000000000, 0.9510565162951535312, 1.000000000000000000, 0.9510565162951535312, 1.000000000000000000, 0.9510565162951535312, 1.000000000000000000, 0.9510565162951535312, 1.000000000000000000, 0.9510565162951535312, 1.000000000000000000, 0.9510565162951535312, 1.000000000000000000, 0.9510565162951535312, 1.000000000000000000, 0.9510565162951535312, 1.000000000000000000, 0.9510565162951535312, 1.000000000000000000, 0.9510565162951535312, 1.000000000000000000, 0.9510565162951535312, 1.000000000000000000, 0.9510565162951535312, 1.000000000000000000, 0.9510565162951535312, 1.000000000000000000, 0.9510565162951535312, 1.000000000000000000, 0.9510565162951535312, 1.000000000000000000, 0.9510565162951535312, 1.000000000000000000, 0.9510565162951535312, 1.000000000000000000, 0.9510565162951535312, 1.000000000000000000, 0.9510565162951535312, 1.000000000000000000, 0.9510565162951535312, 1.000000000000000000, 0.9510565162951535312, 1.000000000000000000, 0.9510565162951535312, 1.000000000000000000, 0.9510565162951535312, 1.000000000000000000, 0.9510565162951535312, 1.000000000000000000, 0.9510565162951535312, 1.000000000000000000, 0.9510565162951535312, 1.000000000000000000, 0.9510565162951535312, 1.000000000000000000, 0.9510565162951535312, 1.000000000000000000, 0.9510565162951535312, 1.000000000000000000, 0.9510565162951535312, 1.000000000000000000, 0.9510565162951535312, 1.000000000000000000, 0.9510565162951535312, 1.000000000000000000, 0.9510565162951535312, 1.000000000000000000, 0.9510565162951535312, 1.000000000000000000, 0.9510565162951535312, 1.000000000000000000, 0.9510565162951535312, 1.000000000000000000, 0.9510565162951535312, 1.000000000000000000, 0.9510565162951535312, 1.000000000000000000, 0.9510565162951535312, 1.000000000000000000, 0.9510565162951535312, 1.000000000000000000, 0.9510565162951535312, 1.000000000000000000, 0.9510565162951535312, 1.000000000000000000, 0.9510565162951535312, 1.000000000000000000, 0.9510565162951535312, 1.000000000000000000, 0.9510565162951535312, 1.000000000000000000, 0.9510565162951535312, 1.000000000000000000, 0.9510565162951535312, 1.000000000000000000, 0.9510565162951535312, 1.000000000000000000, 0.9510565162951535312, 1.000000000000000000, 0.9510565162951535312, 1.000000000000000000, 0.9510565162951535312, 1.000000000000000000, 0.9510565162951535312, 1.000000000000000000, 0.9510565162951535312, 1.000000000000000000, 0.9510565162951535312, 1.000000000000000000, 0.9510565162951535312, 1.000000000000000000, 0.9510565162951535312, 1.000000000000000000, 0.9510565162951535312, 1.000000000000000000, 0.9510565162951535312, 1.000000000000000000, 0.9510565162951535312, 1.000000000000000000, 0.9510565162951535312, 1.000000000000000000, 0.9510565162951535312, 1.000000000000000000, 0.9510565162951535312, 1.000000000000000000, 0.9510565162951535312, 1.000000000000000000, 0.9510565162951535312, 1.000000000000000000, 0.9510565162951535312, 1.000000000000000000, 0.9510565162951535312, 1.000000000000000000, 0.9510565162951535312, 1.000000000000000000, 0.9510565162951535312, 1.000000000000000000, 0.9510565162951535312, 1.000000000000000000, 0.9510565162951535312, 1.000000000000000000, 0.9510565162951535312, 1.000000000000000000, 0.9510565162951535312, 1.000000000000000000, 0.9510565162951535312, 1.000000000000000000, 0.9510565162951535312, 1.000000000000000000, 0.9510565162951535312, 1.000000000000000000, 0.9510565162951535312, 1.000000000000000000, 0.9510565162951535312, 1.000000000000000000, 0.9510565162951535312, 1.000000000000000000, 0.9510565162951535312, 1.000000000000000000, 0.9510565162951535312, 1.000000000000000000, 0.9510565162951535312, 1.000000000000000000, 0.9510565162951535312, 1.000000000000000000, 0.9510565162951535312, 1.000000000000000000, 0.9510565162951535312, 1.000000000000000000, 0.9510565162951535312, 1.000000000000000000, 0.9510565162951535312, 1.000000000000000000, 0.9510565162951535312, 1.000000000000000000, 0.9510565162951535312, 1.000000000000000000, 0.9510565162951535312, 1.000000000000000000, 0.9510565162951535312, 1.000000000000000000, 0.9510565162951535312, 1.000000000000000000, 0.9510565162951535312, 1.000000000000000000, 0.9510565162951535312, 1.000000000000000000, 0.9510565162951535312, 1.000000000000000000, 0.9510565162951535312, 1.000000000000000000, 0.9510565162951535312, 1.000000000000000000, 0.9510565162951535312, 1.000000000000000000, 0.9510565162951535312, 1.000000000000000000, 0.9510565162951535312, 1.000000000000000000, 0.9510565162951535312, 1.000000000000000000, 0.9510565162951535312, 1.000000000000000000, 0.9510565162951535312, 1.000000000000000000, 0.9510565162951535312, 1.000000000000000000, 0.9510565162951535312, 1.000000000000000000, 0.9510565162951535312, 1.000000000000000000, 0.9510565162951535312, 1.000000000000000000, 0.9510565162951535312, 1.000000000000000000, 0.9510565162951535312, 1.000000000000000000, 0.9510565162951535312, 1.000000000000000000, 0.9510565162951535312, 1.000000000000000000, 0.9510565162951535312, 1.000000000000000000, 0.9510565162951535312, 1.000000000000000000, 0.9510565162951535312, 1.000000000000000000, 0.9510565162951535312, 1.000000000000000000, 0.9510565162951535312, 1.000000000000000000, 0.9510565162951535312, 1.000000000000000000, 0.9510565162951535312, 1.000000000000000000, 0.9510565162951535312, 1.000000000000000000, 0.9510565162951535312, 1.000000000000000000, 0.9510565162951535312, 1.000000000000000000, 0.9510565162951535312, 1.000000000000000000, 0.9510565162951535312, 1.000000000000000000, 0.9510565162951535312, 1.000000000000000000, 0.9510565162951535312, 1.000000000000000000, 0.9510565162951535312, 1.000000000000000000, 0.9510565162951535312, 1.000000000000000000, 0.9510565162951535312, 1.000000000000000000, 0.9510565162951535312, 1.000000000000000000, 0.9510565162951535312, 1.000000000000000000, 0.9510565162951535312, 1.000000000000000000, 0.9510565162951535312, 1.000000000000000000, 0.9510565162951535312, 1.000000000000000000, 0.9510565162951535312, 1.000000000000000000, 0.9510565162951535312, 1.000000000000000000, 0.9510565162951535312, 1.000000000000000000, 0.9510565162951535312, 1.000000000000000000, 0.9510565162951535312, 1.000000000000000000, 0.9510565162951535312, 1.000000000000000000, 0.9510565162951535312, 1.000000000000000000, 0.9510565162951535312, 1.000000000000000000, 0.9510565162951535312, 1.000000000000000000, 0.9510565162951535312, 1.000000000000000000, 0.9510565162951535312, 1.000000000000000000, 0.9510565162951535312, 1.000000000000000000, 0.9510565162951535312, 1.000000000000000000, 0.9510565162951535312, 1.000000000000000000, 0.9510565162951535312, 1.000000000000000000, 0.9510565162951535312, 1.000000000000000000, 0.9510565162951535312, 1.000000000000000000, 0.9510565162951535312, 1.000000000000000000, 0.9510565162951535312, 1.000000000000000000, 0.9510565162951535312, 1.000000000000000000, 0.9510565162951535312, 1.000000000000000000, 0.9510565162951535312, 1.000000000000000000, 0.9510565162951535312, 1.000000000000000000, 0.9510565162951535312, 1.000000000000000000, 0.9510565162951535312, 1.000000000000000000, 0.9510565162951535312, 1.000000000000000000, 0.9510565162951535312, 1.000000000000000000, 0.9510565162951535312, 1.000000000000000000, 0.9510565162951535312, 1.000000000000000000, 0.9510565162951535312, 1.000000000000000000, 0.9510565162951535312, 1.000000000000000000, 0.9510565162951535312, 1.000000000000000000, 0.9836243115514174962, 0.9782066976764471899),
 ( 1.000000000000000000, 0.9510565162951535312, 1.000000000000000000, 0.9510565162951535312, 1.000000000000000000, 0.9510565162951535312, 1.000000000000000000, 0.9510565162951535312, 1.000000000000000000, 0.9510565162951535312, 1.000000000000000000, 0.9510565162951535312, 1.000000000000000000, 0.9510565162951535312, 1.000000000000000000, 0.9510565162951535312, 1.000000000000000000, 0.9510565162951535312, 1.000000000000000000, 0.9510565162951535312, 1.000000000000000000, 0.9510565162951535312, 1.000000000000000000, 0.9510565162951535312, 1.000000000000000000, 0.9510565162951535312, 1.000000000000000000, 0.9510565162951535312, 1.000000000000000000, 0.9510565162951535312, 1.000000000000000000, 0.9510565162951535312, 1.000000000000000000, 0.9510565162951535312, 1.000000000000000000, 0.9510565162951535312, 1.000000000000000000, 0.9510565162951535312, 1.000000000000000000, 0.9510565162951535312, 1.000000000000000000, 0.9510565162951535312, 1.000000000000000000, 0.9510565162951535312, 1.000000000000000000, 0.9510565162951535312, 1.000000000000000000, 0.9510565162951535312, 1.000000000000000000, 0.9510565162951535312, 1.000000000000000000, 0.9510565162951535312, 1.000000000000000000, 0.9510565162951535312, 1.000000000000000000, 0.9510565162951535312, 1.000000000000000000, 0.9510565162951535312, 1.000000000000000000, 0.9510565162951535312, 1.000000000000000000, 0.9510565162951535312, 1.000000000000000000, 0.9510565162951535312, 1.000000000000000000, 0.9510565162951535312, 1.000000000000000000, 0.9510565162951535312, 1.000000000000000000, 0.9510565162951535312, 1.000000000000000000, 0.9510565162951535312, 1.000000000000000000, 0.9510565162951535312, 1.000000000000000000, 0.9510565162951535312, 1.000000000000000000, 0.9510565162951535312, 1.000000000000000000, 0.9510565162951535312, 1.000000000000000000, 0.9510565162951535312, 1.000000000000000000, 0.9510565162951535312, 1.000000000000000000, 0.9510565162951535312, 1.000000000000000000, 0.9510565162951535312, 1.000000000000000000, 0.9510565162951535312, 1.000000000000000000, 0.9510565162951535312, 1.000000000000000000, 0.9510565162951535312, 1.000000000000000000, 0.9510565162951535312, 1.000000000000000000, 0.9510565162951535312, 1.000000000000000000, 0.9510565162951535312, 1.000000000000000000, 0.9510565162951535312, 1.000000000000000000, 0.9510565162951535312, 1.000000000000000000, 0.9510565162951535312, 1.000000000000000000, 0.9510565162951535312, 1.000000000000000000, 0.9510565162951535312, 1.000000000000000000, 0.9510565162951535312, 1.000000000000000000, 0.9510565162951535312, 1.000000000000000000, 0.9510565162951535312, 1.000000000000000000, 0.9510565162951535312, 1.000000000000000000, 0.9510565162951535312, 1.000000000000000000, 0.9510565162951535312, 1.000000000000000000, 0.9510565162951535312, 1.000000000000000000, 0.9510565162951535312, 1.000000000000000000, 0.9510565162951535312, 1.000000000000000000, 0.9510565162951535312, 1.000000000000000000, 0.9510565162951535312, 1.000000000000000000, 0.9510565162951535312, 1.000000000000000000, 0.9510565162951535312, 1.000000000000000000, 0.9510565162951535312, 1.000000000000000000, 0.9510565162951535312, 1.000000000000000000, 0.9510565162951535312, 1.000000000000000000, 0.9510565162951535312, 1.000000000000000000, 0.9510565162951535312, 1.000000000000000000, 0.9510565162951535312, 1.000000000000000000, 0.9510565162951535312, 1.000000000000000000, 0.9510565162951535312, 1.000000000000000000, 0.9510565162951535312, 1.000000000000000000, 0.9510565162951535312, 1.000000000000000000, 0.9510565162951535312, 1.000000000000000000, 0.9510565162951535312, 1.000000000000000000, 0.9510565162951535312, 1.000000000000000000, 0.9510565162951535312, 1.000000000000000000, 0.9510565162951535312, 1.000000000000000000, 0.9510565162951535312, 1.000000000000000000, 0.9510565162951535312, 1.000000000000000000, 0.9510565162951535312, 1.000000000000000000, 0.9510565162951535312, 1.000000000000000000, 0.9510565162951535312, 1.000000000000000000, 0.9510565162951535312, 1.000000000000000000, 0.9510565162951535312, 1.000000000000000000, 0.9510565162951535312, 1.000000000000000000, 0.9510565162951535312, 1.000000000000000000, 0.9510565162951535312, 1.000000000000000000, 0.9510565162951535312, 1.000000000000000000, 0.9510565162951535312, 1.000000000000000000, 0.9510565162951535312, 1.000000000000000000, 0.9510565162951535312, 1.000000000000000000, 0.9510565162951535312, 1.000000000000000000, 0.9510565162951535312, 1.000000000000000000, 0.9510565162951535312, 1.000000000000000000, 0.9510565162951535312, 1.000000000000000000, 0.9510565162951535312, 1.000000000000000000, 0.9510565162951535312, 1.000000000000000000, 0.9510565162951535312, 1.000000000000000000, 0.9510565162951535312, 1.000000000000000000, 0.9510565162951535312, 1.000000000000000000, 0.9510565162951535312, 1.000000000000000000, 0.9510565162951535312, 1.000000000000000000, 0.9510565162951535312, 1.000000000000000000, 0.9510565162951535312, 1.000000000000000000, 0.9510565162951535312, 1.000000000000000000, 0.9510565162951535312, 1.000000000000000000, 0.9510565162951535312, 1.000000000000000000, 0.9510565162951535312, 1.000000000000000000, 0.9510565162951535312, 1.000000000000000000, 0.9510565162951535312, 1.000000000000000000, 0.9510565162951535312, 1.000000000000000000, 0.9510565162951535312, 1.000000000000000000, 0.9510565162951535312, 1.000000000000000000, 0.9510565162951535312, 1.000000000000000000, 0.9510565162951535312, 1.000000000000000000, 0.9510565162951535312, 1.000000000000000000, 0.9510565162951535312, 1.000000000000000000, 0.9510565162951535312, 1.000000000000000000, 0.9510565162951535312, 1.000000000000000000, 0.9510565162951535312, 1.000000000000000000, 0.9510565162951535312, 1.000000000000000000, 0.9510565162951535312, 1.000000000000000000, 0.9510565162951535312, 1.000000000000000000, 0.9510565162951535312, 1.000000000000000000, 0.9510565162951535312, 1.000000000000000000, 0.9510565162951535312, 1.000000000000000000, 0.9510565162951535312, 1.000000000000000000, 0.9510565162951535312, 1.000000000000000000, 0.9510565162951535312, 1.000000000000000000, 0.9510565162951535312, 1.000000000000000000, 0.9510565162951535312, 1.000000000000000000, 0.9510565162951535312, 1.000000000000000000, 0.9510565162951535312, 1.000000000000000000, 0.9510565162951535312, 1.000000000000000000, 0.9510565162951535312, 1.000000000000000000, 0.9510565162951535312, 1.000000000000000000, 0.9510565162951535312, 1.000000000000000000, 0.9510565162951535312, 1.000000000000000000, 0.9510565162951535312, 1.000000000000000000, 0.9510565162951535312, 1.000000000000000000, 0.9510565162951535312, 1.000000000000000000, 0.9510565162951535312, 1.000000000000000000, 0.9510565162951535312, 1.000000000000000000, 0.9510565162951535312, 1.000000000000000000, 0.9510565162951535312, 1.000000000000000000, 0.9510565162951535312, 1.000000000000000000, 0.9510565162951535312, 1.000000000000000000, 0.9510565162951535312, 1.000000000000000000, 0.9510565162951535312, 1.000000000000000000, 0.9510565162951535312, 1.000000000000000000, 0.9510565162951535312, 1.000000000000000000, 0.9510565162951535312, 1.000000000000000000, 0.9510565162951535312, 1.000000000000000000, 0.9510565162951535312, 1.000000000000000000, 0.9510565162951535312, 1.000000000000000000, 0.9510565162951535312, 1.000000000000000000, 0.9510565162951535312, 1.000000000000000000, 0.9510565162951535312, 1.000000000000000000, 0.9510565162951535312, 1.000000000000000000, 0.9510565162951535312, 1.000000000000000000, 0.9510565162951535312, 1.000000000000000000, 0.9510565162951535312, 1.000000000000000000, 0.9510565162951535312, 1.000000000000000000, 0.9510565162951535312, 1.000000000000000000, 0.9510565162951535312, 1.000000000000000000, 0.9510565162951535312, 1.000000000000000000, 0.9510565162951535312, 1.000000000000000000, 0.9510565162951535312, 1.000000000000000000, 0.9510565162951535312, 1.000000000000000000, 0.9510565162951535312, 1.000000000000000000, 0.9510565162951535312, 1.000000000000000000, 0.9510565162951535312, 1.000000000000000000, 0.9510565162951535312, 1.000000000000000000, 0.9510565162951535312, 1.000000000000000000, 0.9510565162951535312, 1.000000000000000000, 0.9510565162951535312, 1.000000000000000000, 0.9510565162951535312, 1.000000000000000000, 0.9510565162951535312, 1.000000000000000000, 0.9510565162951535312, 1.000000000000000000, 0.9510565162951535312, 1.000000000000000000, 0.9510565162951535312, 1.000000000000000000, 0.9510565162951535312, 1.000000000000000000, 0.9510565162951535312, 1.000000000000000000, 0.9510565162951535312, 1.000000000000000000, 0.9510565162951535312, 1.000000000000000000, 0.9510565162951535312, 1.000000000000000000, 0.9510565162951535312, 1.000000000000000000, 0.9510565162951535312, 1.000000000000000000, 0.9510565162951535312, 1.000000000000000000, 0.9510565162951535312, 1.000000000000000000, 0.9510565162951535312, 1.000000000000000000, 0.9510565162951535312, 1.000000000000000000, 0.9510565162951535312, 1.000000000000000000, 0.9510565162951535312, 1.000000000000000000, 0.9510565162951535312, 1.000000000000000000, 0.9510565162951535312, 1.000000000000000000, 0.9510565162951535312, 1.000000000000000000, 0.9510565162951535312, 1.000000000000000000, 0.9510565162951535312, 1.000000000000000000, 0.9510565162951535312, 1.000000000000000000, 0.9510565162951535312, 1.000000000000000000, 0.9510565162951535312, 1.000000000000000000, 0.9510565162951535312, 1.000000000000000000, 0.9510565162951535312, 1.000000000000000000, 0.9510565162951535312, 1.000000000000000000, 0.9510565162951535312, 1.000000000000000000, 0.9510565162951535312, 1.000000000000000000, 0.9510565162951535312, 1.000000000000000000, 0.9510565162951535312, 1.000000000000000000, 0.9510565162951535312, 1.000000000000000000, 0.9510565162951535312, 1.000000000000000000, 0.9510565162951535312, 1.000000000000000000, 0.9510565162951535312, 1.000000000000000000, 0.9510565162951535312, 1.000000000000000000, 0.9510565162951535312, 1.000000000000000000, 0.9510565162951535312, 1.000000000000000000, 0.9510565162951535312, 1.000000000000000000, 0.9510565162951535312, 1.000000000000000000, 0.9510565162951535312, 1.000000000000000000, 0.9510565162951535312, 1.000000000000000000, 0.9510565162951535312, 1.000000000000000000, 0.9510565162951535312, 1.000000000000000000, 0.9510565162951535312, 1.000000000000000000, 0.9510565162951535312, 1.000000000000000000, 0.9510565162951535312, 1.000000000000000000, 0.9510565162951535312, 1.000000000000000000, 0.9510565162951535312, 1.000000000000000000, 0.9510565162951535312, 1.000000000000000000, 0.9510565162951535312, 1.000000000000000000, 0.9510565162951535312, 1.000000000000000000, 0.9510565162951535312, 1.000000000000000000, 0.9510565162951535312, 1.000000000000000000, 0.9510565162951535312, 1.000000000000000000, 0.9510565162951535312, 1.000000000000000000, 0.9510565162951535312, 1.000000000000000000, 0.9510565162951535312, 1.000000000000000000, 0.9510565162951535312, 1.000000000000000000, 0.9510565162951535312, 1.000000000000000000, 0.9510565162951535312, 1.000000000000000000, 0.9510565162951535312, 1.000000000000000000, 0.9510565162951535312, 1.000000000000000000, 0.9510565162951535312, 1.000000000000000000, 0.9510565162951535312, 1.000000000000000000, 0.9510565162951535312, 1.000000000000000000, 0.9510565162951535312, 1.000000000000000000, 0.9510565162951535312, 1.000000000000000000, 0.9510565162951535312, 1.000000000000000000, 0.9510565162951535312, 1.000000000000000000, 0.9510565162951535312, 1.000000000000000000, 0.9510565162951535312, 1.000000000000000000, 0.9510565162951535312, 1.000000000000000000, 0.9510565162951535312, 1.000000000000000000, 0.9510565162951535312, 1.000000000000000000, 0.9510565162951535312, 1.000000000000000000, 0.9510565162951535312, 1.000000000000000000, 0.9510565162951535312, 1.000000000000000000, 0.9510565162951535312, 1.000000000000000000, 0.9510565162951535312, 1.000000000000000000, 0.9510565162951535312, 1.000000000000000000, 0.9510565162951535312, 1.000000000000000000, 0.9510565162951535312, 1.000000000000000000, 0.9510565162951535312, 1.000000000000000000, 0.9510565162951535312, 1.000000000000000000, 0.9510565162951535312, 1.000000000000000000, 0.9510565162951535312, 1.000000000000000000, 0.9510565162951535312, 1.000000000000000000, 0.9510565162951535312, 1.000000000000000000, 0.9510565162951535312, 1.000000000000000000, 0.9510565162951535312, 1.000000000000000000, 0.9510565162951535312, 1.000000000000000000, 0.9510565162951535312, 1.000000000000000000, 0.9510565162951535312, 1.000000000000000000, 0.9510565162951535312, 1.000000000000000000, 0.9510565162951535312, 1.000000000000000000, 0.9510565162951535312, 1.000000000000000000, 0.9510565162951535312, 1.000000000000000000, 0.9510565162951535312, 1.000000000000000000, 0.9510565162951535312, 1.000000000000000000, 0.9510565162951535312, 1.000000000000000000, 0.9510565162951535312, 1.000000000000000000, 0.9510565162951535312, 1.000000000000000000, 0.9510565162951535312, 1.000000000000000000, 0.9510565162951535312, 1.000000000000000000, 0.9510565162951535312, 1.000000000000000000, 0.9510565162951535312, 1.000000000000000000, 0.9510565162951535312, 1.000000000000000000, 0.9510565162951535312, 1.000000000000000000, 0.9510565162951535312, 1.000000000000000000, 0.9510565162951535312, 1.000000000000000000, 0.9510565162951535312, 1.000000000000000000, 0.9510565162951535312, 1.000000000000000000, 0.9510565162951535312, 1.000000000000000000, 0.9510565162951535312, 1.000000000000000000, 0.9510565162951535312, 1.000000000000000000, 0.9510565162951535312, 1.000000000000000000, 0.9510565162951535312, 1.000000000000000000, 0.9510565162951535312, 1.000000000000000000, 0.9510565162951535312, 1.000000000000000000, 0.9510565162951535312, 1.000000000000000000, 0.9510565162951535312, 1.000000000000000000, 0.9510565162951535312, 1.000000000000000000, 0.9510565162951535312, 1.000000000000000000, 0.9510565162951535312, 1.000000000000000000, 0.9510565162951535312, 1.000000000000000000, 0.9510565162951535312, 1.000000000000000000, 0.9510565162951535312, 1.000000000000000000, 0.9510565162951535312, 1.000000000000000000, 0.9510565162951535312, 1.000000000000000000, 0.9510565162951535312, 1.000000000000000000, 0.9510565162951535312, 1.000000000000000000, 0.9510565162951535312, 1.000000000000000000, 0.9510565162951535312, 1.000000000000000000, 0.9510565162951535312, 1.000000000000000000, 0.9510565162951535312, 1.000000000000000000, 0.9510565162951535312, 1.000000000000000000, 0.9510565162951535312, 1.000000000000000000, 0.9510565162951535312, 1.000000000000000000, 0.9510565162951535312, 1.000000000000000000, 0.9510565162951535312, 1.000000000000000000, 0.9510565162951535312, 1.000000000000000000, 0.9510565162951535312, 1.000000000000000000, 0.9510565162951535312, 1.000000000000000000, 0.9510565162951535312, 1.000000000000000000, 0.9510565162951535312, 1.000000000000000000, 0.9510565162951535312, 1.000000000000000000, 0.9510565162951535312, 1.000000000000000000, 0.9510565162951535312, 1.000000000000000000, 0.9836243115514174962, 0.9782066976764471899) ) ) 
 REPRESENTATION_ITEM ( '' )  SURFACE ( )  );
#18544 = CARTESIAN_POINT ( 'NONE',  ( 38.58424406990784661, 77.96518717409396970, 32.77220824515698183 ) ) ;
#18545 = CARTESIAN_POINT ( 'NONE',  ( 42.21948215057684450, 81.03738109496902098, 29.21067981925356705 ) ) ;
#18546 = DIRECTION ( 'NONE',  ( -0.8731411001063289490, 0.4874675571821265319, 0.000000000000000000 ) ) ;
#18547 = ORIENTED_EDGE ( 'NONE', *, *, #2884, .T. ) ;
#18548 = CARTESIAN_POINT ( 'NONE',  ( 41.64333658814960870, 60.97977050742731109, 38.42115945441014446 ) ) ;
#18549 = CARTESIAN_POINT ( 'NONE',  ( -151.4692556286852891, -182.9084106276440025, 39.74470866294723947 ) ) ;
#18550 = AXIS2_PLACEMENT_3D ( 'NONE', #3740, #8816, #15206 ) ;
#18551 = CARTESIAN_POINT ( 'NONE',  ( 69.91774837562090283, 98.61087038541865013, -1.665158713316885919 ) ) ;
#18552 = CARTESIAN_POINT ( 'NONE',  ( -145.6429501568359797, -174.2084106276440423, 41.63779006702063867 ) ) ;
#18553 = ORIENTED_EDGE ( 'NONE', *, *, #5368, .F. ) ;
#18554 = CARTESIAN_POINT ( 'NONE',  ( 43.01140435219951286, 156.8651871740940180, 38.86567161673127657 ) ) ;
#18555 =( GEOMETRIC_REPRESENTATION_CONTEXT ( 3 ) GLOBAL_UNCERTAINTY_ASSIGNED_CONTEXT ( ( #20551 ) ) GLOBAL_UNIT_ASSIGNED_CONTEXT ( ( #19886, #2908, #19543 ) ) REPRESENTATION_CONTEXT ( 'NONE', 'WORKASPACE' ) );
#18556 = CARTESIAN_POINT ( 'NONE',  ( -141.4692556286852891, -159.9891397928654726, 49.65701158161630957 ) ) ;
#18557 = CARTESIAN_POINT ( 'NONE',  ( 43.01140435219951286, 115.1297705074272955, 38.86567161673127657 ) ) ;
#18558 = CARTESIAN_POINT ( 'NONE',  ( 8.927628897234525240, 116.7075971571176751, 1.981832035706394546 ) ) ;
#18559 = ORIENTED_EDGE ( 'NONE', *, *, #16479, .T. ) ;
#18560 = CARTESIAN_POINT ( 'NONE',  ( 24.69269415895541542, 98.46806607146707790, -5.796035312751787849 ) ) ;
#18561 = VERTEX_POINT ( 'NONE', #20 ) ;
#18562 = LINE ( 'NONE', #1587, #18537 ) ;
#18563 = CARTESIAN_POINT ( 'NONE',  ( 45.74753988029933538, 158.0651871740940067, 30.44471234641811819 ) ) ;
#18564 = AXIS2_PLACEMENT_3D ( 'NONE', #7833, #16297, #7938 ) ;
#18565 = CARTESIAN_POINT ( 'NONE',  ( 77.16427934405430733, 119.9933672671919851, 6.581674455321548933 ) ) ;
#18566 = CARTESIAN_POINT ( 'NONE',  ( 126.8576204525573274, -126.9891397928655010, -17.64809332337413750 ) ) ;
#18567 = CARTESIAN_POINT ( 'NONE',  ( 156.5268905834513475, 193.0332408774651185, -50.99999999999998579 ) ) ;
#18568 = CARTESIAN_POINT ( 'NONE',  ( -145.2889157411863721, -180.5391397928654555, 41.15050349809590102 ) ) ;
#18569 = CARTESIAN_POINT ( 'NONE',  ( 138.2733499813809885, 177.2661675079481540, -44.99999999999997158 ) ) ;
#18570 = FACE_OUTER_BOUND ( 'NONE', #3999, .T. ) ;
#18571 = FACE_OUTER_BOUND ( 'NONE', #16966, .T. ) ;
#18572 = ITEM_DEFINED_TRANSFORMATION ( 'NONE', 'NONE', #9159,  #12657 ) ;
#18573 = CARTESIAN_POINT ( 'NONE',  ( 46.59305225739526435, 94.57977050742731251, 36.81289934271958941 ) ) ;
#18574 = CARTESIAN_POINT ( 'NONE',  ( 53.00431643774457768, 93.53749527547704190, -6.986323292181506162 ) ) ;
#18575 = CARTESIAN_POINT ( 'NONE',  ( -142.0420953463935803, -174.2438272943107052, 46.59394152635518793 ) ) ;
#18576 = CARTESIAN_POINT ( 'NONE',  ( 44.37947211624943833, 79.01518717409400949, 38.42115945441014446 ) ) ;
#18577 = AXIS2_PLACEMENT_3D ( 'NONE', #16805, #15158, #7012 ) ;
#18578 = CARTESIAN_POINT ( 'NONE',  ( -145.2889157411863437, -195.5391397928654271, 41.15050349809589392 ) ) ;
#18579 = ORIENTED_EDGE ( 'NONE', *, *, #19622, .F. ) ;
#18580 = CARTESIAN_POINT ( 'NONE',  ( 39.92123440845005433, 138.2344580088725650, 38.46393386101375711 ) ) ;
#18581 = CARTESIAN_POINT ( 'NONE',  ( 59.73150498404358899, 90.03452709159309109, 13.76780503130795097 ) ) ;
#18582 = CARTESIAN_POINT ( 'NONE',  ( 39.42975644700377558, 138.6797705074273210, 36.81289934271958941 ) ) ;
#18583 = CARTESIAN_POINT ( 'NONE',  ( 25.97839122281734703, 97.53232036182296838, 2.136956866322798021 ) ) ;
#18584 = VECTOR ( 'NONE', #18005, 1000.000000000000000 ) ;
#18585 = CARTESIAN_POINT ( 'NONE',  ( 39.42975644700377558, 60.67977050742731393, 36.81289934271958941 ) ) ;
#18586 = EDGE_LOOP ( 'NONE', ( #18326, #3438, #3202, #5552 ) ) ;
#18587 = CARTESIAN_POINT ( 'NONE',  ( 38.58424406990786082, 144.3797705074273097, 34.21067981925357060 ) ) ;
#18588 = EDGE_CURVE ( 'NONE', #4997, #19976, #3550, .T. ) ;
#18589 = CARTESIAN_POINT ( 'NONE',  ( 38.58424406990784661, 96.52977050742730114, 35.64915139335016647 ) ) ;
#18590 = CARTESIAN_POINT ( 'NONE',  ( 39.92123440845005433, 142.1604996726487400, 38.46393386101375711 ) ) ;
#18591 = AXIS2_PLACEMENT_3D ( 'NONE', #3283, #86, #13527 ) ;
#18592 = DIRECTION ( 'NONE',  ( 0.000000000000000000, 1.000000000000000000, 0.000000000000000000 ) ) ;
#18593 = CARTESIAN_POINT ( 'NONE',  ( -159.5594255724347761, -169.2630981290892862, 55.53486410454104316 ) ) ;
#18594 = LINE ( 'NONE', #16925, #11519 ) ;
#18595 = CARTESIAN_POINT ( 'NONE',  ( -151.4692556286852607, -167.3130981290893260, 39.65701158161629536 ) ) ;
#18596 = CARTESIAN_POINT ( 'NONE',  ( -159.5594255724347761, -166.2630981290893146, 55.53486410454104316 ) ) ;
#18597 = VECTOR ( 'NONE', #13386, 1000.000000000000000 ) ;
#18598 = DIRECTION ( 'NONE',  ( 0.000000000000000000, -1.000000000000000000, 0.000000000000000000 ) ) ;
#18599 = CARTESIAN_POINT ( 'NONE',  ( 38.96631938032478359, 144.0844580088725877, 37.14960608071593384 ) ) ;
#18600 = CARTESIAN_POINT ( 'NONE',  ( 47.43856463449118621, 127.8797705074273239, 34.21067981925357060 ) ) ;
#18601 = CARTESIAN_POINT ( 'NONE',  ( 41.36127970224624306, 91.67401929561202678, -0.5144393322287174053 ) ) ;
#18602 = CARTESIAN_POINT ( 'NONE',  ( 39.92123440845005433, 141.2344580088725365, 38.46393386101375711 ) ) ;
#18603 = CARTESIAN_POINT ( 'NONE',  ( 47.43856463449117911, 115.7651871740939953, 32.77220824515697473 ) ) ;
#18604 = ADVANCED_FACE ( 'NONE', ( #16978 ), #3109, .T. ) ;
#18605 = CARTESIAN_POINT ( 'NONE',  ( 42.21948215057684450, 126.4575765865522925, 39.21067981925355639 ) ) ;
#18606 = CARTESIAN_POINT ( 'NONE',  ( 22.17150742865759483, 138.9041494244890771, -4.010207742755246052 ) ) ;
#18607 = CARTESIAN_POINT ( 'NONE',  ( -141.4692556286852891, -185.9130981290892919, 46.40781461928724383 ) ) ;
#18608 = CARTESIAN_POINT ( 'NONE',  ( 47.43856463449118621, 85.87977050742730967, 34.21067981925357060 ) ) ;
#18609 = ORIENTED_EDGE ( 'NONE', *, *, #9863, .T. ) ;
#18610 = CARTESIAN_POINT ( 'NONE',  ( -143.3790856849358306, -167.7630981290893146, 43.77915905869157598 ) ) ;
#18611 = CARTESIAN_POINT ( 'NONE',  ( 44.55648932407425633, 72.68445800887258201, 38.96596240072933170 ) ) ;
#18612 = CARTESIAN_POINT ( 'NONE',  ( -27.64582385433944367, -84.13255853780189852, 5.000000000000018652 ) ) ;
#18613 = CARTESIAN_POINT ( 'NONE',  ( 46.10157429594899270, 134.6604996726487684, 29.95742577749337343 ) ) ;
#18615 = CARTESIAN_POINT ( 'NONE',  ( 23.54274795406405474, 91.84646939011692268, -11.98975411606233976 ) ) ;
#18614 = CARTESIAN_POINT ( 'NONE',  ( 41.64333658814960870, 83.51518717409400949, 30.00020018409699318 ) ) ;
#18616 = EDGE_CURVE ( 'NONE', #15249, #10801, #16722, .T. ) ;
#18617 = CARTESIAN_POINT ( 'NONE',  ( -159.5594255724347761, -194.7891397928654555, 43.77915905869157598 ) ) ;
#18618 = CARTESIAN_POINT ( 'NONE',  ( -157.2955611005345986, -178.4438272943107222, 57.67623309621197336 ) ) ;
#18619 = CYLINDRICAL_SURFACE ( 'NONE', #11467, 4.999999999999997335 ) ;
#18620 = FACE_OUTER_BOUND ( 'NONE', #5004, .T. ) ;
#18621 = CARTESIAN_POINT ( 'NONE',  ( 43.01140435219957681, 93.53445800887259054, 39.21067981925356349 ) ) ;
#18622 = CARTESIAN_POINT ( 'NONE',  ( 43.80332655382221674, 142.5373810949690210, 39.21067981925356349 ) ) ;
#18623 = CARTESIAN_POINT ( 'NONE',  ( 47.43856463449117200, 151.7297705074273324, 35.64915139335016647 ) ) ;
#18624 = CARTESIAN_POINT ( 'NONE',  ( -161.4692556286853176, -184.5630981290892976, 49.65701158161630957 ) ) ;
#18625 = CARTESIAN_POINT ( 'NONE',  ( 65.27013532398795803, 145.9152199903044504, 11.62486143609835310 ) ) ;
#18626 = CARTESIAN_POINT ( 'NONE',  ( 47.43856463449118621, 142.6151871740939896, 34.21067981925357060 ) ) ;
#18627 = CARTESIAN_POINT ( 'NONE',  ( -148.5561028927606344, -156.9938272943107052, 58.62277379824867296 ) ) ;
#18628 = CARTESIAN_POINT ( 'NONE',  ( -160.8964159109769696, -179.1584106276440309, 49.65701158161630957 ) ) ;
#18629 = CIRCLE ( 'NONE', #668, 10.00000000000003730 ) ;
#18630 = CARTESIAN_POINT ( 'NONE',  ( 41.64333658814960870, 62.51518717409400239, 30.00020018409699318 ) ) ;
#18631 = CARTESIAN_POINT ( 'NONE',  ( -159.0959885057557983, -161.4584106276440423, 44.11586579668791330 ) ) ;
#18632 = CARTESIAN_POINT ( 'NONE',  ( 46.46425003030392986, 147.9761360841216344, 3.056716434341200106 ) ) ;
#18633 = SURFACE_SIDE_STYLE ('',( #117 ) ) ;
#18634 = CARTESIAN_POINT ( 'NONE',  ( 44.37947211624943833, 124.0151871740939953, 38.42115945441014446 ) ) ;
#18635 = ORIENTED_EDGE ( 'NONE', *, *, #1438, .F. ) ;
#18636 = ORIENTED_EDGE ( 'NONE', *, *, #10169, .T. ) ;
#18637 = CARTESIAN_POINT ( 'NONE',  ( 43.01140435219951286, 146.0344580088725479, 29.21067981925356705 ) ) ;
#18638 = VERTEX_POINT ( 'NONE', #10060 ) ;
#18639 = ADVANCED_FACE ( 'NONE', ( #3448 ), #13360, .T. ) ;
#18640 = CARTESIAN_POINT ( 'NONE',  ( 46.10157429594899270, 97.73445800887256496, 29.95742577749337343 ) ) ;
#18641 = CARTESIAN_POINT ( 'NONE',  ( 46.59305225739526435, 155.1797705074273210, 31.60846029578754468 ) ) ;
#18642 = CIRCLE ( 'NONE', #7067, 10.00000000000000888 ) ;
#18643 = CARTESIAN_POINT ( 'NONE',  ( 39.42975644700377558, 60.07977050742731251, 31.60846029578754468 ) ) ;
#18645 = CARTESIAN_POINT ( 'NONE',  ( 69.05514009256096131, 130.5101840208823205, -14.76775785107876082 ) ) ;
#18644 = CARTESIAN_POINT ( 'NONE',  ( 40.27526882409969033, 116.6651871740939868, 30.44471234641811819 ) ) ;
#18646 = CARTESIAN_POINT ( 'NONE',  ( 41.46631938032478359, 85.31049967264874567, 38.96596240072933170 ) ) ;
#18647 = CARTESIAN_POINT ( 'NONE',  ( 43.80332655382220253, 148.9575765865523067, 29.21067981925356705 ) ) ;
#18648 = CARTESIAN_POINT ( 'NONE',  ( 43.01140435219957681, 97.46049967264875136, 39.21067981925356349 ) ) ;
#18649 = CARTESIAN_POINT ( 'NONE',  ( -159.5594255724347761, -190.8630981290893089, 43.77915905869157598 ) ) ;
#18650 = CARTESIAN_POINT ( 'NONE',  ( 41.64333658814960870, 80.51518717409400949, 30.00020018409699318 ) ) ;
#18651 = DIRECTION ( 'NONE',  ( 0.000000000000000000, 0.000000000000000000, 1.000000000000000000 ) ) ;
#18652 = CARTESIAN_POINT ( 'NONE',  ( 47.05648932407426344, 126.9844580088725934, 37.14960608071593384 ) ) ;
#18653 = CARTESIAN_POINT ( 'NONE',  ( 116.4417310231185780, -126.9891397928655010, 0.3429884183836981459 ) ) ;
#18654 = ORIENTED_EDGE ( 'NONE', *, *, #4689, .T. ) ;
#18655 = CARTESIAN_POINT ( 'NONE',  ( -157.2955611005346270, -190.7084106276440423, 57.67623309621198047 ) ) ;
#18656 = CARTESIAN_POINT ( 'NONE',  ( 70.62757080055673953, 99.67629488849819097, 13.29148015538516425 ) ) ;
#18657 = CARTESIAN_POINT ( 'NONE',  ( -160.8964159109769696, -173.3084106276440366, 46.59394152635518793 ) ) ;
#18658 = ORIENTED_EDGE ( 'NONE', *, *, #11961, .F. ) ;
#18659 = EDGE_CURVE ( 'NONE', #2272, #1525, #828, .T. ) ;
#18660 = CARTESIAN_POINT ( 'NONE',  ( 46.59305225739526435, 157.3151871740940067, 36.81289934271958941 ) ) ;
#18661 = CARTESIAN_POINT ( 'NONE',  ( 45.74753988029933538, 100.1651871740939868, 37.97664729208901946 ) ) ;
#18662 = CARTESIAN_POINT ( 'NONE',  ( -55.11860757350579831, 784.8075632535900468, -3.999999999999996447 ) ) ;
#18663 = CARTESIAN_POINT ( 'NONE',  ( 45.74753988029934249, 116.3297705074273125, 30.44471234641812174 ) ) ;
#18664 = CARTESIAN_POINT ( 'NONE',  ( 36.38086904327614235, 86.32171732562966326, 0.5532606071062302622 ) ) ;
#18665 = ORIENTED_EDGE ( 'NONE', *, *, #15930, .F. ) ;
#18666 = CARTESIAN_POINT ( 'NONE',  ( 58.35211712195835076, 96.24552883246097679, -7.224606741634919338 ) ) ;
#18667 = VERTEX_POINT ( 'NONE', #17194 ) ;
#18668 = CARTESIAN_POINT ( 'NONE',  ( 40.27526882409969033, 111.8297705074272983, 37.97664729208901946 ) ) ;
#18669 = CARTESIAN_POINT ( 'NONE',  ( 38.01140435219952707, 158.7844580088725763, 34.21067981925357060 ) ) ;
#18670 = DIRECTION ( 'NONE',  ( -0.000000000000000000, 1.000000000000000000, -0.000000000000000000 ) ) ;
#18671 = CARTESIAN_POINT ( 'NONE',  ( 39.42975644700377558, 141.4151871740940010, 36.81289934271958941 ) ) ;
#18672 =( BOUNDED_CURVE ( )  B_SPLINE_CURVE ( 2, ( #21441, #11725, #5017, #16567, #18459, #19898, #8218, #19670, #4564, #13282, #2917, #20017, #13057 ),
 .UNSPECIFIED., .F., .F. ) 
 B_SPLINE_CURVE_WITH_KNOTS ( ( 3, 2, 2, 2, 2, 2, 3 ),
 ( 0.02205882352941176267, 0.02352941176470588203, 0.02647058823529411728, 0.02941176470588235253, 0.03235294117647059126, 0.03529411764705882304, 0.03676470588235294240 ),
 .UNSPECIFIED. ) 
 CURVE ( )  GEOMETRIC_REPRESENTATION_ITEM ( )  RATIONAL_B_SPLINE_CURVE ( ( 0.9755282581475768211, 0.9755282581475768211, 1.000000000000000000, 0.9510565162951535312, 1.000000000000000000, 0.9510565162951535312, 1.000000000000000000, 0.9510565162951535312, 1.000000000000000000, 0.9510565162951535312, 1.000000000000000000, 0.9755282581475768211, 0.9755282581475768211 ) ) 
 REPRESENTATION_ITEM ( '' )  );
#18673 = CARTESIAN_POINT ( 'NONE',  ( 76.97600836722278927, 116.3222765712875031, 6.700797217583226661 ) ) ;
#18674 = AXIS2_PLACEMENT_3D ( 'NONE', #678, #7631, #1005 ) ;
#18675 = DIRECTION ( 'NONE',  ( -0.3450121214752277510, 0.9385982292947088190, 0.000000000000000000 ) ) ;
#18676 = CARTESIAN_POINT ( 'NONE',  ( -161.4692556286852607, -182.3391397928654669, 52.90620854394536821 ) ) ;
#18677 = DIRECTION ( 'NONE',  ( -0.3450121214752274734, 0.9385982292947088190, 0.000000000000000000 ) ) ;
#18678 = LINE ( 'NONE', #15147, #16389 ) ;
#18679 = CARTESIAN_POINT ( 'NONE',  ( 46.10157429594899270, 96.83445800887255928, 38.46393386101375711 ) ) ;
#18680 = CARTESIAN_POINT ( 'NONE',  ( 38.01140435219952707, 98.78445800887259054, 34.21067981925357060 ) ) ;
#18681 = CARTESIAN_POINT ( 'NONE',  ( 44.37947211624943833, 97.27977050742732956, 38.42115945441014446 ) ) ;
#18682 = CARTESIAN_POINT ( 'NONE',  ( 20.57499262110235350, 102.8243204193801432, -5.557751863727047770 ) ) ;
#18683 = CARTESIAN_POINT ( 'NONE',  ( -145.6429501568359797, -170.9438272943107222, 41.63779006702063867 ) ) ;
#18684 = CARTESIAN_POINT ( 'NONE',  ( 43.01140435219951286, 75.86518717409398960, 38.86567161673127657 ) ) ;
#18685 = PLANE ( 'NONE',  #18382 ) ;
#18686 = ORIENTED_EDGE ( 'NONE', *, *, #14025, .F. ) ;
#18687 = ADVANCED_FACE ( 'NONE', ( #15342, #7405 ), #234, .T. ) ;
#18688 = EDGE_CURVE ( 'NONE', #10043, #16938, #19187, .T. ) ;
#18689 = CARTESIAN_POINT ( 'NONE',  ( -141.4692556286852891, -189.8391397928655238, 46.40781461928724383 ) ) ;
#18690 = FACE_OUTER_BOUND ( 'NONE', #10049, .T. ) ;
#18691 = CARTESIAN_POINT ( 'NONE',  ( 47.43856463449117911, 143.0297705074273154, 32.77220824515697473 ) ) ;
#18692 = CARTESIAN_POINT ( 'NONE',  ( 22.77429378292968920, 139.4308542021594519, -2.981927144630473148 ) ) ;
#18693 = VECTOR ( 'NONE', #10584, 1000.000000000000000 ) ;
#18694 = DIRECTION ( 'NONE',  ( 1.387778780781445676E-16, 1.000000000000000000, -0.000000000000000000 ) ) ;
#18695 = ORIENTED_EDGE ( 'NONE', *, *, #11352, .T. ) ;
#18696 = CARTESIAN_POINT ( 'NONE',  ( 39.42975644700377558, 135.0797705074272983, 31.60846029578754468 ) ) ;
#18697 = CARTESIAN_POINT ( 'NONE',  ( 46.59305225739526435, 100.5797705074273267, 36.81289934271958941 ) ) ;
#18698 = CARTESIAN_POINT ( 'NONE',  ( -157.6495955161842062, -193.1130981290893089, 58.16351966513671812 ) ) ;
#18699 = LINE ( 'NONE', #13834, #13955 ) ;
#18700 = FACE_OUTER_BOUND ( 'NONE', #7720, .T. ) ;
#18701 = CARTESIAN_POINT ( 'NONE',  ( -141.4692556286852891, -174.0630981290893260, 49.65701158161630957 ) ) ;
#18702 = CARTESIAN_POINT ( 'NONE',  ( 41.46631938032478359, 123.3844580088725849, 38.96596240072933170 ) ) ;
#18703 = CARTESIAN_POINT ( 'NONE',  ( -143.3790856849358306, -164.7630981290893146, 43.77915905869157598 ) ) ;
#18704 = CARTESIAN_POINT ( 'NONE',  ( -151.4692556286852891, -189.2391397928654726, 39.65701158161630246 ) ) ;
#18705 = CARTESIAN_POINT ( 'NONE',  ( 46.10157429594899270, 138.8344580088725877, 38.46393386101376421 ) ) ;
#18706 = CARTESIAN_POINT ( 'NONE',  ( 45.74753988029933538, 119.3297705074273267, 30.44471234641811819 ) ) ;
#18707 = CARTESIAN_POINT ( 'NONE',  ( 69.60802376816022274, 110.2920722108499518, -1.943010761821444943 ) ) ;
#18708 = CARTESIAN_POINT ( 'NONE',  ( -149.8854112254399240, -183.3160212151857422, 39.65701158161629536 ) ) ;
#18709 = CARTESIAN_POINT ( 'NONE',  ( 39.42975644700377558, 105.4151871740940152, 36.81289934271958941 ) ) ;
#18710 = LINE ( 'NONE', #1954, #7678 ) ;
#18711 = CARTESIAN_POINT ( 'NONE',  ( 34.64294707643933435, 153.0196542278736729, 4.557659493426334585 ) ) ;
#18712 = CARTESIAN_POINT ( 'NONE',  ( 24.69269415895541542, 98.46806607146707790, -5.796035312751787849 ) ) ;
#18713 = CARTESIAN_POINT ( 'NONE',  ( -148.3790856849358306, -186.6630981290893203, 59.16757674456786020 ) ) ;
#18714 = CARTESIAN_POINT ( 'NONE',  ( 40.27526882409969744, 84.82977050742732672, 37.97664729208901235 ) ) ;
#18715 = VERTEX_POINT ( 'NONE', #10815 ) ;
#18716 = CARTESIAN_POINT ( 'NONE',  ( 43.01140435219951996, 10.71049967264875491, 34.21067981925357060 ) ) ;
#18717 = CARTESIAN_POINT ( 'NONE',  ( 38.96631938032478359, 68.48445800887257917, 31.27175355779120025 ) ) ;
#18718 = CARTESIAN_POINT ( 'NONE',  ( 43.01140435219951996, 10.71049967264875491, 39.21067981925356349 ) ) ;
#18719 = CARTESIAN_POINT ( 'NONE',  ( 48.01140435219951996, 131.2104996726487514, 34.21067981925357060 ) ) ;
#18721 = CARTESIAN_POINT ( 'NONE',  ( 11.90670198672629354, 134.0117795012786814, -10.44205992529839122 ) ) ;
#18720 = CARTESIAN_POINT ( 'NONE',  ( 45.74753988029933538, 91.16518717409397254, 37.97664729208901946 ) ) ;
#18722 = CARTESIAN_POINT ( 'NONE',  ( -145.2889157411863721, -195.5391397928654555, 41.15050349809590102 ) ) ;
#18723 = CARTESIAN_POINT ( 'NONE',  ( -160.8964159109769696, -178.7438272943106767, 52.72008163687743121 ) ) ;
#18724 = CARTESIAN_POINT ( 'NONE',  ( 38.01140435219952707, 93.86049967264874283, 35.83527830041809636 ) ) ;
#18725 = CARTESIAN_POINT ( 'NONE',  ( 20.98687704487253569, 141.7792436784441747, -11.00219731500033049 ) ) ;
#18726 = VECTOR ( 'NONE', #889, 1000.000000000000000 ) ;
#18727 = APPLICATION_CONTEXT ( 'automotive_design' ) ;
#18728 = VECTOR ( 'NONE', #15099, 1000.000000000000000 ) ;
#18729 = CARTESIAN_POINT ( 'NONE',  ( 11.17254549292281673, -61.68114226949890622, 20.00000000000001776 ) ) ;
#18730 = CARTESIAN_POINT ( 'NONE',  ( -157.6495955161842062, -173.0391397928654840, 58.16351966513671812 ) ) ;
#18731 = CARTESIAN_POINT ( 'NONE',  ( 47.43856463449117200, 155.0297705074273154, 32.77220824515698183 ) ) ;
#18732 = CARTESIAN_POINT ( 'NONE',  ( 40.27526882409969033, 105.8297705074273125, 37.97664729208901946 ) ) ;
#18733 = CARTESIAN_POINT ( 'NONE',  ( 50.13766412853455279, 153.4730781396112889, -3.927228689826556707 ) ) ;
#18734 = CARTESIAN_POINT ( 'NONE',  ( 43.01140435219951286, 138.8651871740940180, 38.86567161673127657 ) ) ;
#18735 = AXIS2_PLACEMENT_3D ( 'NONE', #11970, #4928, #11639 ) ;
#18736 = CARTESIAN_POINT ( 'NONE',  ( 43.80332655382222384, 67.95757658655230671, 29.21067981925357770 ) ) ;
#18737 = CARTESIAN_POINT ( 'NONE',  ( -159.0959885057557983, -170.4584106276440423, 44.11586579668791330 ) ) ;
#18738 = CARTESIAN_POINT ( 'NONE',  ( 40.27526882409969744, 59.66518717409400097, 30.44471234641812174 ) ) ;
#18739 = CARTESIAN_POINT ( 'NONE',  ( 10.92950091243491251, 131.9893946842779542, 22.49106082041198107 ) ) ;
#18740 = DIRECTION ( 'NONE',  ( 0.000000000000000000, 0.000000000000000000, 1.000000000000000000 ) ) ;
#18741 = CARTESIAN_POINT ( 'NONE',  ( 45.74753988029933538, 112.1651871740939868, 37.97664729208901946 ) ) ;
#18742 = ORIENTED_EDGE ( 'NONE', *, *, #4231, .T. ) ;
#18743 = ORIENTED_EDGE ( 'NONE', *, *, #9886, .T. ) ;
#18744 = CIRCLE ( 'NONE', #2893, 21.90454335994848734 ) ;
#18745 = CARTESIAN_POINT ( 'NONE',  ( -143.3790856849358306, -193.2891397928654555, 55.53486410454105027 ) ) ;
#18746 = ORIENTED_EDGE ( 'NONE', *, *, #16887, .F. ) ;
#18747 = CARTESIAN_POINT ( 'NONE',  ( 41.46631938032478359, 102.3844580088725849, 38.96596240072933170 ) ) ;
#18748 = CARTESIAN_POINT ( 'NONE',  ( 43.01140435219951286, 157.1297705074273097, 38.86567161673127657 ) ) ;
#18749 = CARTESIAN_POINT ( 'NONE',  ( 40.27526882409969033, 59.92977050742730682, 30.44471234641811819 ) ) ;
#18751 = CARTESIAN_POINT ( 'NONE',  ( 64.82873087846098770, 102.1656695083886603, -13.57732884656604355 ) ) ;
#18750 = CARTESIAN_POINT ( 'NONE',  ( 44.37947211624943833, 113.2151871740940123, 30.00020018409699318 ) ) ;
#18752 = EDGE_CURVE ( 'NONE', #15773, #5761, #19123, .T. ) ;
#18753 = CARTESIAN_POINT ( 'NONE',  ( 38.96631938032478359, 75.41049967264873999, 31.27175355779120025 ) ) ;
#18755 = DIRECTION ( 'NONE',  ( 1.000000000000000000, 0.000000000000000000, 0.000000000000000000 ) ) ;
#18754 = CARTESIAN_POINT ( 'NONE',  ( 43.01140435219951286, 107.0344580088725763, 29.21067981925356705 ) ) ;
#18756 = CARTESIAN_POINT ( 'NONE',  ( -151.4692556286853176, -174.2391397928654726, 39.65701158161629536 ) ) ;
#18757 = DIRECTION ( 'NONE',  ( -1.000000000000000000, 0.000000000000000000, 0.000000000000000000 ) ) ;
#18758 = CARTESIAN_POINT ( 'NONE',  ( 41.64333658814960870, 81.71518717409399812, 38.42115945441014446 ) ) ;
#18759 = PRODUCT_DEFINITION_CONTEXT ( 'detailed design', #10848, 'design' ) ;
#18760 = DIRECTION ( 'NONE',  ( -0.000000000000000000, -0.000000000000000000, -1.000000000000000000 ) ) ;
#18761 = CARTESIAN_POINT ( 'NONE',  ( -142.0420953463936087, -180.3938272943107108, 49.65701158161630957 ) ) ;
#18762 = VERTEX_POINT ( 'NONE', #18756 ) ;
#18763 = CARTESIAN_POINT ( 'NONE',  ( -160.8964159109769696, -188.3084106276440366, 46.59394152635518793 ) ) ;
#18764 = CARTESIAN_POINT ( 'NONE',  ( 30.18028515090226449, 151.2280014487717779, 17.43780275515692679 ) ) ;
#18765 = CARTESIAN_POINT ( 'NONE',  ( -145.6429501568359797, -177.2084106276440423, 41.63779006702063867 ) ) ;
#18766 = ORIENTED_EDGE ( 'NONE', *, *, #6823, .F. ) ;
#18767 = CARTESIAN_POINT ( 'NONE',  ( 45.74753988029933538, 155.0651871740940067, 30.44471234641811819 ) ) ;
#18768 = CARTESIAN_POINT ( 'NONE',  ( 46.59305225739526435, 157.9151871740940010, 31.60846029578754468 ) ) ;
#18769 = CARTESIAN_POINT ( 'NONE',  ( 40.27526882409969744, 104.9297705074273210, 30.44471234641812174 ) ) ;
#18770 = CARTESIAN_POINT ( 'NONE',  ( 26.13368487350976110, 90.12329638092472806, 0.9106621812756837686 ) ) ;
#18771 = ORIENTED_EDGE ( 'NONE', *, *, #9116, .F. ) ;
#18772 = CARTESIAN_POINT ( 'NONE',  ( 32.38101408406643600, 93.78751416920769657, -6.153149741203968404 ) ) ;
#18773 = ORIENTED_EDGE ( 'NONE', *, *, #17549, .T. ) ;
#18774 = CARTESIAN_POINT ( 'NONE',  ( -142.0420953463936087, -195.6584106276440593, 49.65701158161630957 ) ) ;
#18775 = CARTESIAN_POINT ( 'NONE',  ( 43.01140435219951286, 128.0344580088725479, 29.21067981925356705 ) ) ;
#18776 = CARTESIAN_POINT ( 'NONE',  ( 39.42975644700377558, 84.07977050742732672, 31.60846029578754468 ) ) ;
#18777 = CARTESIAN_POINT ( 'NONE',  ( 46.59305225739526435, 142.9151871740940294, 31.60846029578754468 ) ) ;
#18778 = CARTESIAN_POINT ( 'NONE',  ( 73.40451243997107156, 135.6611253642151098, -1.946480675884423084 ) ) ;
#18779 = CARTESIAN_POINT ( 'NONE',  ( -154.5594255724347761, -166.8891397928654499, 59.16757674456785310 ) ) ;
#18780 = CARTESIAN_POINT ( 'NONE',  ( 43.01140435219951286, 107.0344580088725763, 29.21067981925356705 ) ) ;
#18781 = UNCERTAINTY_MEASURE_WITH_UNIT (LENGTH_MEASURE( 1.000000000000000082E-05 ), #10190, 'distance_accuracy_value', 'NONE');
#18782 = DIRECTION ( 'NONE',  ( -0.9393725726208707050, -0.3428981916074316794, -0.000000000000000000 ) ) ;
#18783 = CARTESIAN_POINT ( 'NONE',  ( 48.01140435219951996, 77.06049967264874567, 35.83527830041809636 ) ) ;
#18784 = EDGE_CURVE ( 'NONE', #17077, #2045, #8945, .T. ) ;
#18785 = CARTESIAN_POINT ( 'NONE',  ( 43.01140435219951286, 82.12977050742730967, 38.86567161673127657 ) ) ;
#18786 = CARTESIAN_POINT ( 'NONE',  ( 35.25059181783574758, 92.79662968204097240, -6.272318425388238694 ) ) ;
#18787 = CARTESIAN_POINT ( 'NONE',  ( -145.6429501568359797, -174.8438272943107279, 57.67623309621198047 ) ) ;
#18788 = EDGE_CURVE ( 'NONE', #15486, #16987, #8570, .T. ) ;
#18789 = CARTESIAN_POINT ( 'NONE',  ( 39.42975644700377558, 80.81518717409400665, 31.60846029578754468 ) ) ;
#18790 = CARTESIAN_POINT ( 'NONE',  ( -130.4480969619997950, -126.9891397928655010, -72.64809332337412684 ) ) ;
#18791 = CARTESIAN_POINT ( 'NONE',  ( -153.0531000319306827, -157.8160212151857422, 59.65701158161631668 ) ) ;
#18792 = ORIENTED_EDGE ( 'NONE', *, *, #16496, .F. ) ;
#18793 = CARTESIAN_POINT ( 'NONE',  ( -151.4692556286852891, -189.2391397928654726, 39.65701158161630246 ) ) ;
#18794 = CARTESIAN_POINT ( 'NONE',  ( -156.4692864601533131, -155.0638355923473455, 40.99677534440144200 ) ) ;
#18795 = CARTESIAN_POINT ( 'NONE',  ( 45.08035905667198762, 147.9511986603014861, 4.994099723559113357 ) ) ;
#18796 = ORIENTED_EDGE ( 'NONE', *, *, #18228, .T. ) ;
#18797 = CARTESIAN_POINT ( 'NONE',  ( 46.59305225739526435, 61.57977050742731251, 36.81289934271958941 ) ) ;
#18798 =( BOUNDED_CURVE ( )  B_SPLINE_CURVE ( 2, ( #5048, #11759, #9797, #14950, #19706, #1519, #11425, #4938, #13197, #8136, #14839, #11541, #6476 ),
 .UNSPECIFIED., .F., .F. ) 
 B_SPLINE_CURVE_WITH_KNOTS ( ( 3, 2, 2, 2, 2, 2, 3 ),
 ( 0.3035714285714286031, 0.3071428571428571619, 0.3142857142857142794, 0.3214285714285714524, 0.3285714285714285698, 0.3357142857142856873, 0.3392857142857142461 ),
 .UNSPECIFIED. ) 
 CURVE ( )  GEOMETRIC_REPRESENTATION_ITEM ( )  RATIONAL_B_SPLINE_CURVE ( ( 0.9755282581475768211, 0.9755282581475769321, 1.000000000000000000, 0.9510565162951535312, 1.000000000000000000, 0.9510565162951535312, 1.000000000000000000, 0.9510565162951535312, 1.000000000000000000, 0.9510565162951535312, 1.000000000000000000, 0.9755282581475769321, 0.9755282581475768211 ) ) 
 REPRESENTATION_ITEM ( '' )  );
#18799 = ORIENTED_EDGE ( 'NONE', *, *, #9010, .F. ) ;
#18800 = CARTESIAN_POINT ( 'NONE',  ( 43.01140435219951286, 136.1297705074273381, 38.86567161673127657 ) ) ;
#18801 = CARTESIAN_POINT ( 'NONE',  ( 47.43856463449117200, 61.46518717409399102, 35.64915139335016647 ) ) ;
#18802 = CARTESIAN_POINT ( 'NONE',  ( -151.4692556286852891, -196.9891397928655010, 49.65701158161630957 ) ) ;
#18803 = CARTESIAN_POINT ( 'NONE',  ( -151.4692556286852891, -126.9891397928655010, 49.65701158161630957 ) ) ;
#18804 = AXIS2_PLACEMENT_3D ( 'NONE', #17627, #20952, #12567 ) ;
#18805 = CARTESIAN_POINT ( 'NONE',  ( 46.59305225739526435, 94.91518717409400097, 31.60846029578754468 ) ) ;
#18806 = CARTESIAN_POINT ( 'NONE',  ( 43.01140435219951996, 10.71049967264875491, 29.21067981925357060 ) ) ;
#18807 = DIRECTION ( 'NONE',  ( 0.3450121214752277510, -0.9385982292947088190, 0.000000000000000000 ) ) ;
#18808 = CARTESIAN_POINT ( 'NONE',  ( -141.4692556286852891, -170.9130981290893203, 46.40781461928724383 ) ) ;
#18809 = DIRECTION ( 'NONE',  ( 1.000000000000000000, 0.000000000000000000, 0.000000000000000000 ) ) ;
#18810 = CARTESIAN_POINT ( 'NONE',  ( 47.05648932407426344, 142.5844580088725877, 31.27175355779120025 ) ) ;
#18811 = CARTESIAN_POINT ( 'NONE',  ( 47.43856463449117200, 124.7297705074273182, 35.64915139335016647 ) ) ;
#18812 = CARTESIAN_POINT ( 'NONE',  ( 53.23527110998836775, 93.53878102080766155, -0.9907194398206048414 ) ) ;
#18813 = PLANE ( 'NONE',  #10988 ) ;
#18814 = CARTESIAN_POINT ( 'NONE',  ( 45.74753988029934249, 103.1651871740940152, 37.97664729208901235 ) ) ;
#18815 = DIRECTION ( 'NONE',  ( 0.000000000000000000, 1.000000000000000000, 0.000000000000000000 ) ) ;
#18816 = CARTESIAN_POINT ( 'NONE',  ( 18.86674891209846905, 143.9013856721611546, -11.04182128657428485 ) ) ;
#18817 = CARTESIAN_POINT ( 'NONE',  ( 48.35156950851215640, 92.21792820573091376, 14.20396468032920012 ) ) ;
#18818 = CARTESIAN_POINT ( 'NONE',  ( -143.3790856849358306, -156.3630981290893089, 55.53486410454105027 ) ) ;
#18819 = CARTESIAN_POINT ( 'NONE',  ( 44.37947211624943833, 86.47977050742731819, 30.00020018409699318 ) ) ;
#18820 = VECTOR ( 'NONE', #14834, 1000.000000000000000 ) ;
#18821 = ORIENTED_EDGE ( 'NONE', *, *, #14318, .F. ) ;
#18822 = CARTESIAN_POINT ( 'NONE',  ( 43.01140435219954838, 133.4604996726487514, 39.21067981925356349 ) ) ;
#18823 = CARTESIAN_POINT ( 'NONE',  ( 38.01140435219951996, 71.63445800887258486, 32.58608133808903773 ) ) ;
#18824 = DIRECTION ( 'NONE',  ( 1.000000000000000000, 0.000000000000000000, -0.000000000000000000 ) ) ;
#18825 = EDGE_CURVE ( 'NONE', #9693, #9727, #10018, .T. ) ;
#18826 = CARTESIAN_POINT ( 'NONE',  ( 38.01140435219951996, 132.8604996726487286, 35.83527830041810347 ) ) ;
#18828 = CARTESIAN_POINT ( 'NONE',  ( 43.31828379119179573, 154.0590585871367750, -16.15632009132952973 ) ) ;
#18827 = CARTESIAN_POINT ( 'NONE',  ( 45.74753988029933538, 88.16518717409397254, 37.97664729208901946 ) ) ;
#18829 = CARTESIAN_POINT ( 'NONE',  ( -142.0420953463935803, -156.8084106276440366, 52.72008163687743831 ) ) ;
#18830 = CARTESIAN_POINT ( 'NONE',  ( -157.2955611005345986, -185.3438272943106995, 41.63779006702063867 ) ) ;
#18831 = CARTESIAN_POINT ( 'NONE',  ( -151.4692556286853176, -193.7391397928655010, 59.65701158161632378 ) ) ;
#18832 = LINE ( 'NONE', #427, #9676 ) ;
#18833 = CARTESIAN_POINT ( 'NONE',  ( -54.92240467314265828, 790.2067769114943303, -23.16745088979876499 ) ) ;
#18834 = CARTESIAN_POINT ( 'NONE',  ( 42.21948215057684450, 92.11133943119284595, 29.21067981925356705 ) ) ;
#18835 = DIRECTION ( 'NONE',  ( 0.000000000000000000, 0.000000000000000000, 1.000000000000000000 ) ) ;
#18836 = CARTESIAN_POINT ( 'NONE',  ( 40.27526882409969033, 153.8297705074273267, 37.97664729208901946 ) ) ;
#18837 = CARTESIAN_POINT ( 'NONE',  ( 38.58424406990786082, 102.3797705074273381, 34.21067981925357060 ) ) ;
#18838 = CARTESIAN_POINT ( 'NONE',  ( 21.43032318156618388, 146.4805633285969861, 10.07716523980869816 ) ) ;
#18839 = CARTESIAN_POINT ( 'NONE',  ( 46.59305225739526435, 139.9151871740940010, 31.60846029578754468 ) ) ;
#18840 = CARTESIAN_POINT ( 'NONE',  ( -151.4692556286852891, -189.2391397928654726, 39.65701158161630246 ) ) ;
#18841 = CARTESIAN_POINT ( 'NONE',  ( -154.3824083646099439, -167.7584106276440536, 40.69124936498395328 ) ) ;
#18842 = CARTESIAN_POINT ( 'NONE',  ( 43.01140435219951286, 90.53445800887257633, 39.21067981925356349 ) ) ;
#18843 = CARTESIAN_POINT ( 'NONE',  ( 58.57740969237692497, 96.29577388269515836, -1.228997851713355072 ) ) ;
#18844 = CARTESIAN_POINT ( 'NONE',  ( 41.46631938032478359, 135.3844580088725706, 38.96596240072933170 ) ) ;
#18845 = CARTESIAN_POINT ( 'NONE',  ( 38.58424406990784661, 114.2651871740940095, 35.64915139335016647 ) ) ;
#18846 = VERTEX_POINT ( 'NONE', #3874 ) ;
#18847 = FACE_OUTER_BOUND ( 'NONE', #18224, .T. ) ;
#18848 = EDGE_LOOP ( 'NONE', ( #18077, #2953, #18868, #7750 ) ) ;
#18849 = CARTESIAN_POINT ( 'NONE',  ( 47.05648932407426344, 102.9844580088725792, 37.14960608071593384 ) ) ;
#18850 = EDGE_CURVE ( 'NONE', #13802, #19216, #10599, .T. ) ;
#18851 = CARTESIAN_POINT ( 'NONE',  ( 47.43856463449117911, 152.0297705074273438, 32.77220824515697473 ) ) ;
#18852 = CARTESIAN_POINT ( 'NONE',  ( 47.05648932407426344, 154.9104996726487400, 37.14960608071593384 ) ) ;
#18854 = CARTESIAN_POINT ( 'NONE',  ( 40.94005093944240059, 91.86375568685591020, -12.50564155961141566 ) ) ;
#18853 = CARTESIAN_POINT ( 'NONE',  ( 43.01140435219951286, 114.8651871740939754, 38.86567161673127657 ) ) ;
#18855 = CARTESIAN_POINT ( 'NONE',  ( 48.01140435219951996, 71.06049967264871725, 35.83527830041810347 ) ) ;
#18857 = CARTESIAN_POINT ( 'NONE',  ( 43.01140435219951286, 135.5344580088725763, 39.21067981925356349 ) ) ;
#18856 = CARTESIAN_POINT ( 'NONE',  ( -158.9748091281504401, -116.9891397928655010, 36.65701158161628115 ) ) ;
#18858 = AXIS2_PLACEMENT_3D ( 'NONE', #7108, #13813, #20337 ) ;
#18859 = CARTESIAN_POINT ( 'NONE',  ( 39.92123440845005433, 72.23445800887256496, 38.46393386101375711 ) ) ;
#18860 = CARTESIAN_POINT ( 'NONE',  ( 47.97879638358897836, 95.40545967527941684, 33.55330648861601617 ) ) ;
#18861 = CARTESIAN_POINT ( 'NONE',  ( 43.01140435219951286, 77.36518717409400381, 29.55568802177586463 ) ) ;
#18862 = DIRECTION ( 'NONE',  ( -0.000000000000000000, -0.000000000000000000, 1.000000000000000000 ) ) ;
#18863 = CARTESIAN_POINT ( 'NONE',  ( -142.0420953463935803, -177.5438272943107165, 52.72008163687743831 ) ) ;
#18864 = LINE ( 'NONE', #3661, #7125 ) ;
#18865 = ORIENTED_EDGE ( 'NONE', *, *, #3207, .F. ) ;
#18866 = CARTESIAN_POINT ( 'NONE',  ( -148.5561028927606344, -186.0584106276440650, 40.69124936498395328 ) ) ;
#18867 = CARTESIAN_POINT ( 'NONE',  ( 62.84376099716368458, 92.00366499689042143, 13.64888190966157566 ) ) ;
#18868 = ORIENTED_EDGE ( 'NONE', *, *, #7891, .T. ) ;
#18869 = CARTESIAN_POINT ( 'NONE',  ( 44.37947211624943833, 148.0151871740940237, 38.42115945441014446 ) ) ;
#18870 = CIRCLE ( 'NONE', #7616, 21.90454335994854063 ) ;
#18871 = CARTESIAN_POINT ( 'NONE',  ( 43.01140435219951286, 91.46049967264873715, 39.21067981925356349 ) ) ;
#18872 = CARTESIAN_POINT ( 'NONE',  ( 40.27526882409969744, 101.9297705074273068, 30.44471234641812174 ) ) ;
#18873 = CARTESIAN_POINT ( 'NONE',  ( 14.15704070161504369, 138.3271338521546454, 9.720138693322796897 ) ) ;
#18874 = ORIENTED_EDGE ( 'NONE', *, *, #16016, .F. ) ;
#18875 = CARTESIAN_POINT ( 'NONE',  ( 34.07414013685151843, 93.16113583794900421, 7.775673839875955728 ) ) ;
#18876 = VECTOR ( 'NONE', #18694, 1000.000000000000000 ) ;
#18877 = ORIENTED_EDGE ( 'NONE', *, *, #364, .F. ) ;
#18878 = PLANE ( 'NONE',  #2972 ) ;
#18879 = CARTESIAN_POINT ( 'NONE',  ( 38.96631938032478359, 127.0104996726487343, 37.14960608071593384 ) ) ;
#18880 = CARTESIAN_POINT ( 'NONE',  ( 45.74753988029933538, 148.1651871740940010, 37.97664729208901946 ) ) ;
#18881 = CARTESIAN_POINT ( 'NONE',  ( 46.10157429594899270, 104.6604996726487116, 29.95742577749337343 ) ) ;
#18882 = CARTESIAN_POINT ( 'NONE',  ( 74.85601106972485752, 107.3429126181175661, -0.9942341299615756745 ) ) ;
#18883 = CARTESIAN_POINT ( 'NONE',  ( 42.21948215057684450, 61.38361825032846752, 39.21067981925355639 ) ) ;
#18884 = ADVANCED_FACE ( 'NONE', ( #21387 ), #14646, .F. ) ;
#18885 = CARTESIAN_POINT ( 'NONE',  ( -148.3790856849358306, -171.3891397928654499, 40.14644641866477315 ) ) ;
#18886 = DIRECTION ( 'NONE',  ( 0.000000000000000000, 1.000000000000000000, 0.000000000000000000 ) ) ;
#18887 = CARTESIAN_POINT ( 'NONE',  ( -157.6495955161842062, -194.0391397928653987, 58.16351966513671812 ) ) ;
#18888 = CARTESIAN_POINT ( 'NONE',  ( 43.80332655382220253, 64.95757658655230671, 29.21067981925356705 ) ) ;
#18889 = DIRECTION ( 'NONE',  ( 0.000000000000000000, -1.000000000000000000, 0.000000000000000000 ) ) ;
#18890 = AXIS2_PLACEMENT_3D ( 'NONE', #2679, #7879, #11494 ) ;
#18891 = CARTESIAN_POINT ( 'NONE',  ( 39.42975644700377558, 84.67977050742732104, 36.81289934271958941 ) ) ;
#18892 = CARTESIAN_POINT ( 'NONE',  ( -142.0420953463936087, -177.3938272943107393, 49.65701158161630957 ) ) ;
#18893 = CARTESIAN_POINT ( 'NONE',  ( 47.43856463449117911, 79.76518717409400949, 32.77220824515697473 ) ) ;
#18894 = CARTESIAN_POINT ( 'NONE',  ( -153.0531000319306827, -169.8160212151857138, 59.65701158161631668 ) ) ;
#18895 = PRODUCT_DEFINITION ( 'UNKNOWN', '', #9864, #18759 ) ;
#18896 = CARTESIAN_POINT ( 'NONE',  ( -176.9699209214867608, 72.84679049016736485, -35.00000000000000000 ) ) ;
#18897 = ORIENTED_EDGE ( 'NONE', *, *, #7768, .T. ) ;
#18898 = CARTESIAN_POINT ( 'NONE',  ( 42.21948215057684450, 69.45757658655230671, 39.21067981925355639 ) ) ;
#18899 = CARTESIAN_POINT ( 'NONE',  ( 43.01140435219951286, 83.96049967264873715, 29.21067981925356705 ) ) ;
#18900 = CARTESIAN_POINT ( 'NONE',  ( 46.59305225739526435, 131.1797705074273210, 31.60846029578754468 ) ) ;
#18901 = CARTESIAN_POINT ( 'NONE',  ( 59.05508021657500706, 143.0007772151335814, 5.589501426708507026 ) ) ;
#18902 = ORIENTED_EDGE ( 'NONE', *, *, #11208, .T. ) ;
#18903 = ADVANCED_FACE ( 'NONE', ( #7836 ), #14432, .T. ) ;
#18904 = FACE_OUTER_BOUND ( 'NONE', #11850, .T. ) ;
#18905 = ORIENTED_EDGE ( 'NONE', *, *, #10518, .F. ) ;
#18906 = VECTOR ( 'NONE', #1315, 1000.000000000000227 ) ;
#18907 = CARTESIAN_POINT ( 'NONE',  ( 40.27526882409969033, 131.9297705074273210, 30.44471234641811819 ) ) ;
#18909 = EDGE_CURVE ( 'NONE', #19332, #1684, #16143, .T. ) ;
#18908 = CARTESIAN_POINT ( 'NONE',  ( -149.8854112254399240, -181.6622583705451746, 59.65701158161632378 ) ) ;
#18910 = CARTESIAN_POINT ( 'NONE',  ( 43.01140435219951286, 60.86518717409400381, 38.86567161673127657 ) ) ;
#18911 = DIRECTION ( 'NONE',  ( 0.9609212714474144601, 0.2768218020313508165, 0.000000000000000000 ) ) ;
#18912 = CARTESIAN_POINT ( 'NONE',  ( -148.3790856849358306, -191.4630981290893317, 40.14644641866477315 ) ) ;
#18913 = ADVANCED_FACE ( 'NONE', ( #9167, #883 ), #17950, .F. ) ;
#18914 = VECTOR ( 'NONE', #2891, 1000.000000000000114 ) ;
#18915 = CARTESIAN_POINT ( 'NONE',  ( 38.58424406990786082, 93.11518717409400381, 34.21067981925357060 ) ) ;
#18916 = CARTESIAN_POINT ( 'NONE',  ( 76.17254549292280785, -61.68114226949890622, 20.00000000000000355 ) ) ;
#18917 = DIRECTION ( 'NONE',  ( 0.000000000000000000, 1.000000000000000000, 0.000000000000000000 ) ) ;
#18918 = CARTESIAN_POINT ( 'NONE',  ( -148.3790856849358306, -168.6630981290892919, 59.16757674456786020 ) ) ;
#18919 = CARTESIAN_POINT ( 'NONE',  ( 0.000000000000000000, 0.000000000000000000, 0.000000000000000000 ) ) ;
#18920 = CARTESIAN_POINT ( 'NONE',  ( 47.05648932407426344, 144.9844580088725934, 37.14960608071593384 ) ) ;
#18921 = CARTESIAN_POINT ( 'NONE',  ( 43.01140435219951286, 118.1297705074273097, 38.86567161673127657 ) ) ;
#18922 = CARTESIAN_POINT ( 'NONE',  ( 20.64193819951031017, 102.6032774297415102, 0.4378519886423143381 ) ) ;
#18923 = FACE_OUTER_BOUND ( 'NONE', #17994, .T. ) ;
#18924 = CARTESIAN_POINT ( 'NONE',  ( 46.59305225739526435, 109.9151871740940010, 31.60846029578754468 ) ) ;
#18925 = ADVANCED_FACE ( 'NONE', ( #9492 ), #7622, .F. ) ;
#18926 = AXIS2_PLACEMENT_3D ( 'NONE', #15146, #1707, #12266 ) ;
#18927 = ORIENTED_EDGE ( 'NONE', *, *, #7316, .T. ) ;
#18928 = CARTESIAN_POINT ( 'NONE',  ( 43.01140435219951286, 156.5344580088725479, 39.21067981925355639 ) ) ;
#18929 = CARTESIAN_POINT ( 'NONE',  ( 42.00398509169406935, 85.76881261499585207, 8.367275628961508005 ) ) ;
#18930 =( BOUNDED_CURVE ( )  B_SPLINE_CURVE ( 2, ( #17221, #18888, #10735, #20871, #7328, #2241, #12599, #14353, #5540, #17655, #12267, #15891, #19002 ),
 .UNSPECIFIED., .F., .F. ) 
 B_SPLINE_CURVE_WITH_KNOTS ( ( 3, 2, 2, 2, 2, 2, 3 ),
 ( 0.9191176470588234837, 0.9205882352941175961, 0.9235294117647059320, 0.9264705882352941568, 0.9294117647058823817, 0.9323529411764706065, 0.9338235294117647189 ),
 .UNSPECIFIED. ) 
 CURVE ( )  GEOMETRIC_REPRESENTATION_ITEM ( )  RATIONAL_B_SPLINE_CURVE ( ( 0.9755282581475768211, 0.9755282581475768211, 1.000000000000000000, 0.9510565162951535312, 1.000000000000000000, 0.9510565162951535312, 1.000000000000000000, 0.9510565162951535312, 1.000000000000000000, 0.9510565162951535312, 1.000000000000000000, 0.9755282581475768211, 0.9755282581475768211 ) ) 
 REPRESENTATION_ITEM ( '' )  );
#18931 = CARTESIAN_POINT ( 'NONE',  ( 39.35338560254503903, 91.94623120232463975, 14.56122079753911081 ) ) ;
#18932 = CARTESIAN_POINT ( 'NONE',  ( -130.4480969619997950, -136.9891397928655010, -72.64809332337412684 ) ) ;
#18933 = EDGE_CURVE ( 'NONE', #15277, #12363, #1101, .T. ) ;
#18934 = CARTESIAN_POINT ( 'NONE',  ( 45.74753988029934249, 89.32977050742732672, 30.44471234641812174 ) ) ;
#18935 = ORIENTED_EDGE ( 'NONE', *, *, #18825, .T. ) ;
#18936 = ADVANCED_FACE ( 'NONE', ( #4618 ), #6274, .T. ) ;
#18937 = CARTESIAN_POINT ( 'NONE',  ( 43.01140435219951286, 77.03445800887259054, 28.95336869806222779 ) ) ;
#18938 = CARTESIAN_POINT ( 'NONE',  ( -40.97538603781489996, -6.141859983696321912, -19.99999999999997513 ) ) ;
#18939 = CARTESIAN_POINT ( 'NONE',  ( 48.01140435219951996, 134.3604996726487570, 32.58608133808903773 ) ) ;
#18941 = CARTESIAN_POINT ( 'NONE',  ( 22.73392375623628681, 139.3438357627746882, 11.01889030017397531 ) ) ;
#18940 = CARTESIAN_POINT ( 'NONE',  ( 41.64333658814960870, 87.71518717409399812, 38.42115945441014446 ) ) ;
#18942 = CARTESIAN_POINT ( 'NONE',  ( -161.4692556286852607, -194.6391397928654783, 46.40781461928724383 ) ) ;
#18943 = CARTESIAN_POINT ( 'NONE',  ( -151.4692556286852891, -184.1438272943107108, 59.56931450028537256 ) ) ;
#18944 = CARTESIAN_POINT ( 'NONE',  ( 42.21948215057684450, 93.03738109496902098, 29.21067981925356705 ) ) ;
#18945 = CARTESIAN_POINT ( 'NONE',  ( 43.80332655382220253, 127.9575765865522925, 29.21067981925356705 ) ) ;
#18946 = CARTESIAN_POINT ( 'NONE',  ( 42.21948215057684450, 81.45757658655229250, 39.21067981925355639 ) ) ;
#18947 = CARTESIAN_POINT ( 'NONE',  ( 44.55648932407425633, 67.61049967264872862, 38.96596240072933170 ) ) ;
#18948 = CARTESIAN_POINT ( 'NONE',  ( 101.4021762516569822, 137.5714195593754710, -19.99999999999997868 ) ) ;
#18949 = CARTESIAN_POINT ( 'NONE',  ( 43.01140435219951286, 101.6297705074273239, 29.55568802177586463 ) ) ;
#18950 = CARTESIAN_POINT ( 'NONE',  ( 59.73150498404358899, 90.03452709159309109, 13.76780503130795097 ) ) ;
#18951 = CARTESIAN_POINT ( 'NONE',  ( 47.43856463449117911, 133.7651871740939669, 32.77220824515697473 ) ) ;
#18952 = CARTESIAN_POINT ( 'NONE',  ( -154.5594255724347761, -187.8891397928654783, 59.16757674456785310 ) ) ;
#18953 = CARTESIAN_POINT ( 'NONE',  ( -154.3824083646099439, -164.7584106276440536, 40.69124936498395328 ) ) ;
#18954 = CARTESIAN_POINT ( 'NONE',  ( 40.27526882409969033, 63.82977050742731961, 37.97664729208901946 ) ) ;
#18955 = DIRECTION ( 'NONE',  ( 0.9999746145782334450, -0.007125320983191549967, 0.000000000000000000 ) ) ;
#18956 = CARTESIAN_POINT ( 'NONE',  ( 24.36338960932843634, 98.64599907776933208, 7.223456449276175029 ) ) ;
#18957 = CARTESIAN_POINT ( 'NONE',  ( 43.01140435219951996, 10.71049967264875491, 34.21067981925357060 ) ) ;
#18958 = CARTESIAN_POINT ( 'NONE',  ( 39.42975644700377558, 110.8151871740939924, 31.60846029578754468 ) ) ;
#18959 = EDGE_CURVE ( 'NONE', #12248, #19655, #3350, .T. ) ;
#18960 = ORIENTED_EDGE ( 'NONE', *, *, #16914, .F. ) ;
#18961 = CARTESIAN_POINT ( 'NONE',  ( -161.4692556286853176, -160.5630981290892976, 49.65701158161630957 ) ) ;
#18962 = ORIENTED_EDGE ( 'NONE', *, *, #14722, .T. ) ;
#18963 = CARTESIAN_POINT ( 'NONE',  ( 46.10157429594899270, 105.8344580088725735, 38.46393386101376421 ) ) ;
#18964 = CARTESIAN_POINT ( 'NONE',  ( 45.74753988029934249, 149.3297705074273267, 30.44471234641812174 ) ) ;
#18965 = CARTESIAN_POINT ( 'NONE',  ( 41.64333658814960870, 59.77977050742731535, 30.00020018409699318 ) ) ;
#18967 = CARTESIAN_POINT ( 'NONE',  ( 17.98614708603287937, 106.9092867359673704, 15.63253669370310384 ) ) ;
#18966 = CARTESIAN_POINT ( 'NONE',  ( 43.01140435219951286, 116.3651871740939896, 29.55568802177586463 ) ) ;
#18968 = CARTESIAN_POINT ( 'NONE',  ( 38.96631938032478359, 70.01049967264874851, 37.14960608071593384 ) ) ;
#18970 = CARTESIAN_POINT ( 'NONE',  ( 48.01140435219951996, 136.1344580088725706, 35.83527830041809636 ) ) ;
#18969 = CARTESIAN_POINT ( 'NONE',  ( 101.6431471920911207, 239.2647937927896464, -5.999999999999976019 ) ) ;
#18971 = DIRECTION ( 'NONE',  ( -0.000000000000000000, -0.000000000000000000, 1.000000000000000000 ) ) ;
#18972 = CARTESIAN_POINT ( 'NONE',  ( 43.66822579977166896, 94.91365412844299954, 39.17808643222355869 ) ) ;
#18973 = CARTESIAN_POINT ( 'NONE',  ( 46.59305225739526435, 82.91518717409400097, 31.60846029578754468 ) ) ;
#18974 = DIRECTION ( 'NONE',  ( 1.000000000000000000, 0.000000000000000000, 0.000000000000000000 ) ) ;
#18975 = CARTESIAN_POINT ( 'NONE',  ( -145.6429501568359797, -176.9438272943107506, 41.63779006702063867 ) ) ;
#18976 = DIRECTION ( 'NONE',  ( 1.000000000000000000, 0.000000000000000000, 0.000000000000000000 ) ) ;
#18977 = VERTEX_POINT ( 'NONE', #7513 ) ;
#18978 = CARTESIAN_POINT ( 'NONE',  ( -160.8964159109769696, -179.3084106276440082, 46.59394152635518793 ) ) ;
#18979 = CARTESIAN_POINT ( 'NONE',  ( 8.701189160817120793, 119.3880529461122109, 1.073064441167490557 ) ) ;
#18980 = EDGE_CURVE ( 'NONE', #2626, #9553, #165, .T. ) ;
#18981 = EDGE_LOOP ( 'NONE', ( #21345, #2769, #2771, #15982 ) ) ;
#18982 = CARTESIAN_POINT ( 'NONE',  ( 47.43856463449118621, 145.6151871740939896, 34.21067981925357060 ) ) ;
#18983 = PLANE ( 'NONE',  #18000 ) ;
#18984 = CARTESIAN_POINT ( 'NONE',  ( 46.59305225739526435, 109.5797705074273125, 36.81289934271958941 ) ) ;
#18985 = CARTESIAN_POINT ( 'NONE',  ( 76.66991938639012005, 113.6622739410785670, 5.791450954060403333 ) ) ;
#18986 = VERTEX_POINT ( 'NONE', #4193 ) ;
#18987 = VECTOR ( 'NONE', #2846, 1000.000000000000000 ) ;
#18988 = CARTESIAN_POINT ( 'NONE',  ( 37.56771007382699423, 92.23784766911828115, 0.6328166970475824771 ) ) ;
#18989 =( BOUNDED_CURVE ( )  B_SPLINE_CURVE ( 2, ( #18621, #15426, #7270, #10251, #17384, #15314, #321, #7052, #13757, #20497, #12102, #18834, #3739 ),
 .UNSPECIFIED., .F., .F. ) 
 B_SPLINE_CURVE_WITH_KNOTS ( ( 3, 2, 2, 2, 2, 2, 3 ),
 ( 0.6397058823529411242, 0.6411764705882353477, 0.6441176470588235725, 0.6470588235294117974, 0.6500000000000000222, 0.6529411764705882470, 0.6544117647058823595 ),
 .UNSPECIFIED. ) 
 CURVE ( )  GEOMETRIC_REPRESENTATION_ITEM ( )  RATIONAL_B_SPLINE_CURVE ( ( 0.9755282581475768211, 0.9755282581475758219, 1.000000000000000000, 0.9510565162951535312, 1.000000000000000000, 0.9510565162951535312, 1.000000000000000000, 0.9510565162951535312, 1.000000000000000000, 0.9510565162951535312, 1.000000000000000000, 0.9755282581475768211, 0.9755282581475768211 ) ) 
 REPRESENTATION_ITEM ( '' )  );
#18990 = ORIENTED_EDGE ( 'NONE', *, *, #3935, .F. ) ;
#18991 = CARTESIAN_POINT ( 'NONE',  ( 46.59305225739526435, 112.5797705074273125, 36.81289934271958941 ) ) ;
#18992 = EDGE_CURVE ( 'NONE', #20113, #6422, #106, .T. ) ;
#18993 = PLANE ( 'NONE',  #5945 ) ;
#18994 = CARTESIAN_POINT ( 'NONE',  ( -151.4692556286852891, -126.9891397928655010, -64.65701158161634510 ) ) ;
#18995 = CARTESIAN_POINT ( 'NONE',  ( 44.37947211624943833, 83.47977050742731819, 30.00020018409699318 ) ) ;
#18996 = CARTESIAN_POINT ( 'NONE',  ( 39.42975644700377558, 144.4151871740940294, 36.81289934271958941 ) ) ;
#18997 = CARTESIAN_POINT ( 'NONE',  ( 41.46631938032478359, 97.31049967264873146, 38.96596240072933170 ) ) ;
#18998 = CARTESIAN_POINT ( 'NONE',  ( 9.656473946750173454, 127.6128973189080398, 2.339233609801092406 ) ) ;
#18999 = CARTESIAN_POINT ( 'NONE',  ( -141.4692556286852891, -180.2130981290893033, 52.90620854394536821 ) ) ;
#19000 = CARTESIAN_POINT ( 'NONE',  ( -145.2889157411863721, -165.5391397928654840, 41.15050349809590102 ) ) ;
#19001 = CARTESIAN_POINT ( 'NONE',  ( -176.9699209214867892, -4.918956727831215833E-14, 30.00000000000000000 ) ) ;
#19002 = CARTESIAN_POINT ( 'NONE',  ( 43.01140435219951286, 63.53445800887256922, 39.21067981925356349 ) ) ;
#19003 = CARTESIAN_POINT ( 'NONE',  ( 43.01140435219951286, 107.0344580088725763, 29.21067981925356705 ) ) ;
#19004 = VECTOR ( 'NONE', #16623, 1000.000000000000000 ) ;
#19005 = CARTESIAN_POINT ( 'NONE',  ( 38.58424406990784661, 81.52977050742732956, 35.64915139335016647 ) ) ;
#19006 = CARTESIAN_POINT ( 'NONE',  ( -154.3824083646099439, -163.2938272943107449, 58.62277379824867296 ) ) ;
#19007 = CARTESIAN_POINT ( 'NONE',  ( 45.74753988029934249, 77.06518717409399244, 30.44471234641812174 ) ) ;
#19008 = LINE ( 'NONE', #5545, #11667 ) ;
#19009 = DIRECTION ( 'NONE',  ( -0.000000000000000000, 1.000000000000000000, -0.000000000000000000 ) ) ;
#19010 = ORIENTED_EDGE ( 'NONE', *, *, #5620, .T. ) ;
#19011 = CARTESIAN_POINT ( 'NONE',  ( 38.96631938032478359, 69.08445800887258770, 37.14960608071593384 ) ) ;
#19012 = CARTESIAN_POINT ( 'NONE',  ( -59.65946286876545201, 788.4655180356365918, -19.99999999999997868 ) ) ;
#19013 = CARTESIAN_POINT ( 'NONE',  ( 38.58424406990786082, 129.3797705074273381, 34.21067981925357060 ) ) ;
#19014 = CARTESIAN_POINT ( 'NONE',  ( 70.97434162403952485, 116.9407273601718202, 6.779784368693626995 ) ) ;
#19015 = ORIENTED_EDGE ( 'NONE', *, *, #12154, .T. ) ;
#19016 = FACE_OUTER_BOUND ( 'NONE', #10714, .T. ) ;
#19017 = ADVANCED_FACE ( 'NONE', ( #16738 ), #5650, .F. ) ;
#19018 = VERTEX_POINT ( 'NONE', #4727 ) ;
#19019 = CARTESIAN_POINT ( 'NONE',  ( 40.27526882409969033, 135.8297705074273551, 37.97664729208901946 ) ) ;
#19020 =( GEOMETRIC_REPRESENTATION_CONTEXT ( 3 ) GLOBAL_UNCERTAINTY_ASSIGNED_CONTEXT ( ( #20761 ) ) GLOBAL_UNIT_ASSIGNED_CONTEXT ( ( #14733, #2830, #17706 ) ) REPRESENTATION_CONTEXT ( 'NONE', 'WORKASPACE' ) );
#19021 = CARTESIAN_POINT ( 'NONE',  ( -151.4692556286853176, -180.2391397928654726, 39.65701158161629536 ) ) ;
#19022 = CYLINDRICAL_SURFACE ( 'NONE', #13628, 7.500000000000000000 ) ;
#19023 = CARTESIAN_POINT ( 'NONE',  ( 38.01140435219952707, 129.8604996726487286, 35.83527830041809636 ) ) ;
#19024 = FILL_AREA_STYLE_COLOUR ( '', #20072 ) ;
#19025 = CARTESIAN_POINT ( 'NONE',  ( 41.64333658814960870, 96.71518717409399812, 38.42115945441014446 ) ) ;
#19026 = DIRECTION ( 'NONE',  ( 0.3450121214752278065, -0.9385982292947087080, -0.000000000000000000 ) ) ;
#19027 = CARTESIAN_POINT ( 'NONE',  ( 76.17254549292280785, -61.68114226949890622, -46.21320343559645494 ) ) ;
#19028 = CARTESIAN_POINT ( 'NONE',  ( -141.4692556286852891, -158.9130981290892919, 46.40781461928724383 ) ) ;
#19029 = DIRECTION ( 'NONE',  ( 0.000000000000000000, 0.000000000000000000, 1.000000000000000000 ) ) ;
#19030 = CARTESIAN_POINT ( 'NONE',  ( 38.01140435219951996, 134.6344580088725422, 32.58608133808903773 ) ) ;
#19031 = CARTESIAN_POINT ( 'NONE',  ( 46.59305225739526435, 109.5797705074273125, 36.81289934271958941 ) ) ;
#19032 = CARTESIAN_POINT ( 'NONE',  ( 24.57236314005146838, 141.2733614120550385, -4.872173989822636386 ) ) ;
#19033 = FACE_OUTER_BOUND ( 'NONE', #11035, .T. ) ;
#19034 = CARTESIAN_POINT ( 'NONE',  ( 45.74753988029934249, 110.0651871740939782, 30.44471234641812174 ) ) ;
#19035 = ORIENTED_EDGE ( 'NONE', *, *, #16887, .T. ) ;
#19036 = AXIS2_PLACEMENT_3D ( 'NONE', #19382, #14091, #7283 ) ;
#19037 = CARTESIAN_POINT ( 'NONE',  ( 47.05648932407426344, 139.9104996726487400, 37.14960608071593384 ) ) ;
#19038 = LINE ( 'NONE', #17257, #13995 ) ;
#19039 = CARTESIAN_POINT ( 'NONE',  ( 17.73005198514846725, 142.9879744078657779, -4.089424278207452801 ) ) ;
#19040 = EDGE_CURVE ( 'NONE', #20985, #20856, #4620, .T. ) ;
#19041 = CARTESIAN_POINT ( 'NONE',  ( 14.82803154953497859, 120.8649872489531987, 9.204245268424362081 ) ) ;
#19042 = CYLINDRICAL_SURFACE ( 'NONE', #19542, 10.00000000000000888 ) ;
#19043 = CARTESIAN_POINT ( 'NONE',  ( 40.27526882409969744, 75.82977050742731251, 37.97664729208901235 ) ) ;
#19044 = ORIENTED_EDGE ( 'NONE', *, *, #17326, .T. ) ;
#19045 = CARTESIAN_POINT ( 'NONE',  ( 39.92123440845004723, 62.33445800887258059, 29.95742577749337343 ) ) ;
#19046 = DIRECTION ( 'NONE',  ( 1.000000000000000000, 0.000000000000000000, -0.000000000000000000 ) ) ;
#19047 = CARTESIAN_POINT ( 'NONE',  ( 38.01140435219952707, 126.7104996726487514, 34.21067981925357060 ) ) ;
#19049 = CARTESIAN_POINT ( 'NONE',  ( 53.48172298457406271, 87.39834721931525507, 0.9865115032505324955 ) ) ;
#19048 = CARTESIAN_POINT ( 'NONE',  ( 47.43856463449118621, 76.61518717409400381, 34.21067981925357060 ) ) ;
#19050 = CARTESIAN_POINT ( 'NONE',  ( -143.8425227516148084, -180.0938272943107279, 44.11586579668791330 ) ) ;
#19051 = CARTESIAN_POINT ( 'NONE',  ( 116.4417310231185780, -136.9891397928655010, 49.65701158161629536 ) ) ;
#19052 = CARTESIAN_POINT ( 'NONE',  ( -161.4692556286853176, -190.5630981290892976, 49.65701158161630957 ) ) ;
#19053 = CARTESIAN_POINT ( 'NONE',  ( 41.46631938032478359, 80.18445800887258201, 29.45539723777780239 ) ) ;
#19054 = DIRECTION ( 'NONE',  ( 0.000000000000000000, 0.000000000000000000, 1.000000000000000000 ) ) ;
#19055 = CARTESIAN_POINT ( 'NONE',  ( 137.5268905834513191, 193.0332408774651185, -5.999999999999950262 ) ) ;
#19056 = CARTESIAN_POINT ( 'NONE',  ( 40.27526882409969033, 137.9297705074273210, 30.44471234641811819 ) ) ;
#19057 = CARTESIAN_POINT ( 'NONE',  ( 41.64333658814960870, 105.9797705074273182, 38.42115945441014446 ) ) ;
#19058 = CARTESIAN_POINT ( 'NONE',  ( 28.07864021081662287, 89.10199518432737875, 14.83897397183228861 ) ) ;
#19059 = CARTESIAN_POINT ( 'NONE',  ( 46.59305225739526435, 133.9151871740940010, 31.60846029578754468 ) ) ;
#19060 = CARTESIAN_POINT ( 'NONE',  ( 47.05648932407426344, 67.58445800887258770, 31.27175355779120025 ) ) ;
#19061 = CARTESIAN_POINT ( 'NONE',  ( -160.8964159109769696, -161.3084106276440366, 46.59394152635518083 ) ) ;
#19062 = CARTESIAN_POINT ( 'NONE',  ( 83.67254549292280785, -61.68114226949890622, 30.00000000000000000 ) ) ;
#19063 = CARTESIAN_POINT ( 'NONE',  ( 39.92123440845005433, 136.1604996726487400, 38.46393386101375711 ) ) ;
#19064 = EDGE_CURVE ( 'NONE', #5848, #21236, #14864, .T. ) ;
#19065 = CARTESIAN_POINT ( 'NONE',  ( 20.79828168028384994, 137.4105449198869735, 15.91385929137521771 ) ) ;
#19066 = DIRECTION ( 'NONE',  ( 0.000000000000000000, 0.000000000000000000, 1.000000000000000000 ) ) ;
#19067 = CARTESIAN_POINT ( 'NONE',  ( 40.27526882409969033, 110.6651871740940010, 30.44471234641811819 ) ) ;
#19068 = EDGE_LOOP ( 'NONE', ( #8426, #20422, #9301, #3468 ) ) ;
#19069 = CYLINDRICAL_SURFACE ( 'NONE', #787, 4.999999999999997335 ) ;
#19070 = EDGE_LOOP ( 'NONE', ( #12199, #14364, #19230, #15778, #11268, #9016 ) ) ;
#19071 = CARTESIAN_POINT ( 'NONE',  ( 39.92123440845004723, 93.23445800887256496, 38.46393386101376421 ) ) ;
#19072 = VECTOR ( 'NONE', #7329, 1000.000000000000000 ) ;
#19073 = VECTOR ( 'NONE', #12608, 1000.000000000000114 ) ;
#19074 = CARTESIAN_POINT ( 'NONE',  ( 47.05648932407426344, 157.9104996726487400, 37.14960608071593384 ) ) ;
#19076 = CARTESIAN_POINT ( 'NONE',  ( 15.11514590861459162, 123.4468881749472615, -3.696500957071167104 ) ) ;
#19075 = CARTESIAN_POINT ( 'NONE',  ( 38.58424406990786082, 114.1151871740939896, 34.21067981925357060 ) ) ;
#19077 = CARTESIAN_POINT ( 'NONE',  ( 44.55648932407425633, 71.81049967264874567, 29.45539723777780239 ) ) ;
#19079 = CARTESIAN_POINT ( 'NONE',  ( 44.55648932407425633, 136.8844580088725706, 29.45539723777780239 ) ) ;
#19078 = CARTESIAN_POINT ( 'NONE',  ( 43.01140435219951286, 136.4604996726487514, 39.21067981925356349 ) ) ;
#19080 = CARTESIAN_POINT ( 'NONE',  ( 44.55648932407425633, 82.88445800887257064, 29.45539723777780239 ) ) ;
#19081 = VECTOR ( 'NONE', #18862, 1000.000000000000000 ) ;
#19082 = EDGE_CURVE ( 'NONE', #18246, #18762, #21246, .T. ) ;
#19083 = CARTESIAN_POINT ( 'NONE',  ( 38.96631938032478359, 124.0104996726487343, 37.14960608071593384 ) ) ;
#19084 = CYLINDRICAL_SURFACE ( 'NONE', #3810, 14.42424326798555434 ) ;
#19085 = CARTESIAN_POINT ( 'NONE',  ( 45.74753988029933538, 70.16518717409397254, 37.97664729208901946 ) ) ;
#19086 = CARTESIAN_POINT ( 'NONE',  ( 157.5268905834513475, 193.0332408774651185, -50.99999999999998579 ) ) ;
#19087 = CARTESIAN_POINT ( 'NONE',  ( -154.3824083646099439, -182.4938272943107336, 40.69124936498395328 ) ) ;
#19088 = CARTESIAN_POINT ( 'NONE',  ( -154.3824083646099439, -193.5584106276440650, 58.62277379824867296 ) ) ;
#19089 = ORIENTED_EDGE ( 'NONE', *, *, #11081, .F. ) ;
#19090 = CARTESIAN_POINT ( 'NONE',  ( -143.8425227516148084, -180.9584106276440707, 55.19815736654470584 ) ) ;
#19091 = CARTESIAN_POINT ( 'NONE',  ( 36.57762280775352082, 86.20069522707665044, 6.548861720777491513 ) ) ;
#19092 = EDGE_LOOP ( 'NONE', ( #6902, #2984, #17775, #4528 ) ) ;
#19093 = AXIS2_PLACEMENT_3D ( 'NONE', #10375, #17076, #5723 ) ;
#19094 = CARTESIAN_POINT ( 'NONE',  ( 44.37947211624943833, 142.0151871740939953, 38.42115945441014446 ) ) ;
#19095 = CIRCLE ( 'NONE', #9590, 10.00000000000000888 ) ;
#19096 = CARTESIAN_POINT ( 'NONE',  ( 43.01140435219951996, 149.0344580088725763, 29.21067981925357060 ) ) ;
#19097 = CARTESIAN_POINT ( 'NONE',  ( 39.42975644700377558, 108.6797705074273352, 36.81289934271958941 ) ) ;
#19098 = VERTEX_POINT ( 'NONE', #10033 ) ;
#19099 = ORIENTED_EDGE ( 'NONE', *, *, #6520, .T. ) ;
#19100 = AXIS2_PLACEMENT_3D ( 'NONE', #9648, #6328, #13054 ) ;
#19101 = CARTESIAN_POINT ( 'NONE',  ( 55.81398226145393693, 145.0329042473489096, 4.442248136324586483 ) ) ;
#19102 = ORIENTED_EDGE ( 'NONE', *, *, #14965, .T. ) ;
#19103 = DIRECTION ( 'NONE',  ( 1.000000000000000000, 0.000000000000000000, 0.000000000000000000 ) ) ;
#19104 = CARTESIAN_POINT ( 'NONE',  ( 38.58424406990784661, 81.52977050742732956, 35.64915139335016647 ) ) ;
#19105 = CARTESIAN_POINT ( 'NONE',  ( 44.37947211624943833, 145.0151871740939953, 38.42115945441014446 ) ) ;
#19106 = CARTESIAN_POINT ( 'NONE',  ( 38.01140435219951996, 102.8604996726487286, 35.83527830041810347 ) ) ;
#19107 = CARTESIAN_POINT ( 'NONE',  ( 30.08091612619420729, 88.20954595054467973, -6.232194961517499188 ) ) ;
#19108 = EDGE_CURVE ( 'NONE', #15802, #2795, #18511, .T. ) ;
#19109 = PLANE ( 'NONE',  #21283 ) ;
#19110 = CARTESIAN_POINT ( 'NONE',  ( -161.4692556286852607, -167.3391397928654385, 52.90620854394536821 ) ) ;
#19111 = CARTESIAN_POINT ( 'NONE',  ( 43.01140435219951996, 119.9070776186055838, -19.99999999999997868 ) ) ;
#19112 = LINE ( 'NONE', #10525, #5199 ) ;
#19113 = CARTESIAN_POINT ( 'NONE',  ( 46.10157429594899270, 106.7344580088725650, 29.95742577749336988 ) ) ;
#19114 = EDGE_LOOP ( 'NONE', ( #7697, #3099, #4199, #20325 ) ) ;
#19115 = CARTESIAN_POINT ( 'NONE',  ( 38.58424406990786082, 87.37977050742732388, 34.21067981925357060 ) ) ;
#19116 = CARTESIAN_POINT ( 'NONE',  ( -151.4692556286852891, -164.6438272943107108, 39.74470866294723947 ) ) ;
#19117 = CARTESIAN_POINT ( 'NONE',  ( 45.74753988029934249, 68.06518717409399244, 30.44471234641812174 ) ) ;
#19118 = CARTESIAN_POINT ( 'NONE',  ( 55.11952973528949684, 87.88698225678692211, -7.065691903092018222 ) ) ;
#19119 = CARTESIAN_POINT ( 'NONE',  ( -157.2955611005346270, -193.7084106276440423, 57.67623309621198047 ) ) ;
#19120 = ORIENTED_EDGE ( 'NONE', *, *, #21220, .F. ) ;
#19121 = CARTESIAN_POINT ( 'NONE',  ( 38.96631938032478359, 68.48445800887257917, 31.27175355779120025 ) ) ;
#19122 = DIRECTION ( 'NONE',  ( -1.000000000000000000, 0.000000000000000000, 0.000000000000000000 ) ) ;
#19123 =( BOUNDED_CURVE ( )  B_SPLINE_CURVE ( 2, ( #17517, #15652, #20412, #18859, #5624, #7300, #6974, #2215, #20843, #13678, #5308, #20521, #12346 ),
 .UNSPECIFIED., .F., .F. ) 
 B_SPLINE_CURVE_WITH_KNOTS ( ( 3, 2, 2, 2, 2, 2, 3 ),
 ( 0.8455882352941176405, 0.8470588235294117530, 0.8499999999999999778, 0.8529411764705882026, 0.8558823529411764275, 0.8588235294117646523, 0.8602941176470588758 ),
 .UNSPECIFIED. ) 
 CURVE ( )  GEOMETRIC_REPRESENTATION_ITEM ( )  RATIONAL_B_SPLINE_CURVE ( ( 0.9755282581475768211, 0.9755282581475768211, 1.000000000000000000, 0.9510565162951535312, 1.000000000000000000, 0.9510565162951535312, 1.000000000000000000, 0.9510565162951535312, 1.000000000000000000, 0.9510565162951535312, 1.000000000000000000, 0.9755282581475758219, 0.9755282581475768211 ) ) 
 REPRESENTATION_ITEM ( '' )  );
#19124 = CARTESIAN_POINT ( 'NONE',  ( 47.43856463449118621, 130.8797705074273381, 34.21067981925357060 ) ) ;
#19125 = CARTESIAN_POINT ( 'NONE',  ( 17.95776995827587896, 107.1383635228311846, 9.636927859708212196 ) ) ;
#19126 = ORIENTED_EDGE ( 'NONE', *, *, #15302, .T. ) ;
#19127 = DIRECTION ( 'NONE',  ( 1.000000000000000000, 0.000000000000000000, 0.000000000000000000 ) ) ;
#19128 = ORIENTED_EDGE ( 'NONE', *, *, #19182, .F. ) ;
#19129 = CARTESIAN_POINT ( 'NONE',  ( 46.59305225739526435, 137.1797705074273210, 31.60846029578754468 ) ) ;
#19130 = CYLINDRICAL_SURFACE ( 'NONE', #15029, 10.00000000000000888 ) ;
#19131 = CARTESIAN_POINT ( 'NONE',  ( 163.1446318037170897, 192.3139764232951734, 24.27006575478477757 ) ) ;
#19132 = CARTESIAN_POINT ( 'NONE',  ( 43.01140435219951286, 98.36518717409401802, 29.55568802177586463 ) ) ;
#19133 = CARTESIAN_POINT ( 'NONE',  ( 47.05648932407426344, 132.9844580088725934, 37.14960608071593384 ) ) ;
#19134 = CARTESIAN_POINT ( 'NONE',  ( 136.2768881589198884, 181.8432453435730167, 21.73429951086134082 ) ) ;
#19135 = CARTESIAN_POINT ( 'NONE',  ( -151.4692556286852891, -159.8130981290893260, 60.17163382399899518 ) ) ;
#19136 = DIRECTION ( 'NONE',  ( 1.000000000000000000, 0.000000000000000000, 0.000000000000000000 ) ) ;
#19137 = CARTESIAN_POINT ( 'NONE',  ( 46.10157429594899270, 132.8344580088725593, 38.46393386101376421 ) ) ;
#19138 = CARTESIAN_POINT ( 'NONE',  ( 41.64333658814960870, 110.7797705074273154, 30.00020018409699318 ) ) ;
#19139 = CARTESIAN_POINT ( 'NONE',  ( 66.44170838958859804, 135.7440291252205213, 4.009006963233090026 ) ) ;
#19140 = CARTESIAN_POINT ( 'NONE',  ( -145.6429501568359797, -191.9438272943106938, 41.63779006702063867 ) ) ;
#19141 = CARTESIAN_POINT ( 'NONE',  ( 41.64333658814960870, 104.5151871740939953, 30.00020018409699318 ) ) ;
#19142 = EDGE_LOOP ( 'NONE', ( #18361, #18500, #9087, #10605 ) ) ;
#19143 = CARTESIAN_POINT ( 'NONE',  ( 48.01140435219951996, 76.28445800887257633, 34.21067981925357060 ) ) ;
#19144 = CARTESIAN_POINT ( 'NONE',  ( 14.43535904578935103, 101.2031681353820574, 9.438814132600386486 ) ) ;
#19145 = CARTESIAN_POINT ( 'NONE',  ( 37.00104444766353851, 92.35499785847434850, 7.656504971210453370 ) ) ;
#19146 = PLANE ( 'NONE',  #21675 ) ;
#19147 = CARTESIAN_POINT ( 'NONE',  ( 47.43856463449117911, 73.72977050742731819, 35.64915139335015937 ) ) ;
#19148 = ORIENTED_EDGE ( 'NONE', *, *, #17302, .T. ) ;
#19149 = ORIENTED_EDGE ( 'NONE', *, *, #4788, .T. ) ;
#19150 = CARTESIAN_POINT ( 'NONE',  ( -145.2889157411863437, -164.6130981290893089, 41.15050349809589392 ) ) ;
#19151 = CARTESIAN_POINT ( 'NONE',  ( 48.01140435219951996, 116.3604996726487428, 32.58608133808903773 ) ) ;
#19153 = CARTESIAN_POINT ( 'NONE',  ( 17.06177112331949886, 97.70250936324737268, 2.295960169688653352 ) ) ;
#19152 = CARTESIAN_POINT ( 'NONE',  ( 44.37947211624943833, 77.21518717409399812, 30.00020018409699318 ) ) ;
#19154 = CARTESIAN_POINT ( 'NONE',  ( -159.0959885057557983, -173.1938272943107506, 44.11586579668791330 ) ) ;
#19155 = CARTESIAN_POINT ( 'NONE',  ( 28.07864021081662287, 89.10199518432737875, 14.83897397183228861 ) ) ;
#19156 = CARTESIAN_POINT ( 'NONE',  ( -161.4692556286852607, -190.7130981290893033, 46.40781461928724383 ) ) ;
#19157 = CARTESIAN_POINT ( 'NONE',  ( 42.21948215057684450, 80.11133943119284595, 29.21067981925356705 ) ) ;
#19158 = FACE_BOUND ( 'NONE', #12818, .T. ) ;
#19160 = EDGE_CURVE ( 'NONE', #2815, #1555, #3217, .T. ) ;
#19159 = FACE_OUTER_BOUND ( 'NONE', #625, .T. ) ;
#19161 = CARTESIAN_POINT ( 'NONE',  ( 38.58424406990784661, 141.2297705074273040, 32.77220824515698183 ) ) ;
#19162 = CARTESIAN_POINT ( 'NONE',  ( 69.91774837562090283, 98.61087038541865013, -1.665158713316885919 ) ) ;
#19163 = CARTESIAN_POINT ( 'NONE',  ( 43.01140435219951286, 134.3651871740939612, 29.55568802177586107 ) ) ;
#19164 = CARTESIAN_POINT ( 'NONE',  ( 39.92123440845005433, 70.16049967264873999, 38.46393386101375711 ) ) ;
#19165 = CARTESIAN_POINT ( 'NONE',  ( -142.0420953463935803, -168.5084106276440536, 46.59394152635518083 ) ) ;
#19166 = DIRECTION ( 'NONE',  ( 0.000000000000000000, 1.000000000000000000, 0.000000000000000000 ) ) ;
#19167 = CARTESIAN_POINT ( 'NONE',  ( -130.4480969619998234, -136.9891397928655010, 67.64809332337415526 ) ) ;
#19168 = AXIS2_PLACEMENT_3D ( 'NONE', #16190, #11127, #4508 ) ;
#19169 = CARTESIAN_POINT ( 'NONE',  ( 17.21810733192966936, 108.3100148859214329, 7.699684045823485867 ) ) ;
#19170 = FACE_OUTER_BOUND ( 'NONE', #4426, .T. ) ;
#19171 = CARTESIAN_POINT ( 'NONE',  ( 44.37947211624943833, 119.2151871740939981, 30.00020018409699318 ) ) ;
#19172 = VERTEX_POINT ( 'NONE', #14971 ) ;
#19173 = EDGE_CURVE ( 'NONE', #9746, #21295, #20073, .T. ) ;
#19174 = CARTESIAN_POINT ( 'NONE',  ( 131.8222645499855901, 267.5435007770738025, -6.999999999999995559 ) ) ;
#19175 = ORIENTED_EDGE ( 'NONE', *, *, #18029, .F. ) ;
#19176 = CARTESIAN_POINT ( 'NONE',  ( 44.55648932407425633, 87.68445800887258201, 38.96596240072933170 ) ) ;
#19177 = CARTESIAN_POINT ( 'NONE',  ( 46.59305225739526435, 152.1797705074273210, 31.60846029578754468 ) ) ;
#19178 = ADVANCED_FACE ( 'NONE', ( #8920, #9028, #10679, #12212, #10573 ), #13971, .T. ) ;
#19179 = CARTESIAN_POINT ( 'NONE',  ( 38.96631938032478359, 147.4104996726487400, 31.27175355779120025 ) ) ;
#19181 = CARTESIAN_POINT ( 'NONE',  ( 66.54750331441660194, 135.2948500229566093, -7.982215242636039321 ) ) ;
#19180 = CARTESIAN_POINT ( 'NONE',  ( 44.37947211624943833, 104.2151871740939981, 30.00020018409699318 ) ) ;
#19182 = EDGE_CURVE ( 'NONE', #1468, #17073, #8605, .T. ) ;
#19183 = CARTESIAN_POINT ( 'NONE',  ( 43.01140435219951286, 71.96049967264873715, 28.95336869806222779 ) ) ;
#19185 = CARTESIAN_POINT ( 'NONE',  ( 43.01140435219951286, 62.03445800887256922, 29.21067981925356705 ) ) ;
#19184 = DIRECTION ( 'NONE',  ( -0.3450121214752278065, 0.9385982292947087080, 0.000000000000000000 ) ) ;
#19186 = CARTESIAN_POINT ( 'NONE',  ( -156.1828684652451784, -155.6591478762521206, 41.49287016839741682 ) ) ;
#19187 = LINE ( 'NONE', #4086, #18466 ) ;
#19188 = CYLINDRICAL_SURFACE ( 'NONE', #9446, 10.00000000000000888 ) ;
#19189 = CARTESIAN_POINT ( 'NONE',  ( 38.58424406990784661, 68.96518717409398391, 32.77220824515698183 ) ) ;
#19190 = ADVANCED_FACE ( 'NONE', ( #13651 ), #430, .T. ) ;
#19191 = CARTESIAN_POINT ( 'NONE',  ( -133.8097529055291943, 761.2091818577913500, -19.99999999999997868 ) ) ;
#19192 = CARTESIAN_POINT ( 'NONE',  ( -159.0959885057557983, -181.5938272943107279, 55.19815736654470584 ) ) ;
#19193 = CYLINDRICAL_SURFACE ( 'NONE', #9941, 10.00000000000000888 ) ;
#19194 = ORIENTED_EDGE ( 'NONE', *, *, #9487, .F. ) ;
#19195 = CARTESIAN_POINT ( 'NONE',  ( -142.0420953463935803, -174.8084106276440082, 52.72008163687743831 ) ) ;
#19196 = CARTESIAN_POINT ( 'NONE',  ( 69.75981547520746062, 141.4021063757441823, 10.83457600654633879 ) ) ;
#19197 = VERTEX_POINT ( 'NONE', #17060 ) ;
#19198 = CARTESIAN_POINT ( 'NONE',  ( 46.59305225739526435, 145.3151871740940067, 36.81289934271958941 ) ) ;
#19199 = CARTESIAN_POINT ( 'NONE',  ( 44.37947211624943833, 109.2797705074273154, 38.42115945441014446 ) ) ;
#19200 = ORIENTED_EDGE ( 'NONE', *, *, #15281, .T. ) ;
#19201 = EDGE_LOOP ( 'NONE', ( #15962, #4669, #16155, #18438 ) ) ;
#19202 = EDGE_CURVE ( 'NONE', #5698, #7641, #15739, .T. ) ;
#19203 = CARTESIAN_POINT ( 'NONE',  ( 70.21798013780751546, 127.3226622636268672, -1.629293503064584536 ) ) ;
#19204 = ORIENTED_EDGE ( 'NONE', *, *, #5555, .F. ) ;
#19205 = CARTESIAN_POINT ( 'NONE',  ( 57.67197451322198276, 240.2871645992281628, -6.999999999999982236 ) ) ;
#19206 = VECTOR ( 'NONE', #1618, 1000.000000000000000 ) ;
#19207 = ADVANCED_FACE ( 'NONE', ( #644 ), #2288, .T. ) ;
#19208 = CARTESIAN_POINT ( 'NONE',  ( 46.59305225739526435, 133.3151871740940067, 36.81289934271958941 ) ) ;
#19209 = CARTESIAN_POINT ( 'NONE',  ( 46.10157429594899270, 101.6604996726487542, 29.95742577749337343 ) ) ;
#19210 = CARTESIAN_POINT ( 'NONE',  ( 16.30372524420941716, 141.3216567370616019, 9.839263250375132941 ) ) ;
#19211 = DIRECTION ( 'NONE',  ( 0.000000000000000000, -0.000000000000000000, -1.000000000000000000 ) ) ;
#19212 = CARTESIAN_POINT ( 'NONE',  ( -141.4692556286852891, -171.8391397928654385, 46.40781461928724383 ) ) ;
#19213 = CARTESIAN_POINT ( 'NONE',  ( 41.46631938032478359, 152.1844580088725820, 29.45539723777780239 ) ) ;
#19214 = CARTESIAN_POINT ( 'NONE',  ( 44.55648932407425633, 151.8844580088725991, 29.45539723777780239 ) ) ;
#19215 = CARTESIAN_POINT ( 'NONE',  ( -154.5594255724347761, -162.9630981290893317, 59.16757674456785310 ) ) ;
#19216 = VERTEX_POINT ( 'NONE', #13864 ) ;
#19217 = CARTESIAN_POINT ( 'NONE',  ( 46.59305225739526435, 82.57977050742731251, 36.81289934271958941 ) ) ;
#19218 = CARTESIAN_POINT ( 'NONE',  ( -142.0420953463935803, -162.2438272943107336, 46.59394152635518793 ) ) ;
#19219 = CARTESIAN_POINT ( 'NONE',  ( 38.58424406990786082, 66.11518717409398960, 34.21067981925357060 ) ) ;
#19220 = CARTESIAN_POINT ( 'NONE',  ( 68.88151390383544026, 142.3271613368909811, -9.208263745312144977 ) ) ;
#19221 = CARTESIAN_POINT ( 'NONE',  ( -157.2955611005346270, -191.6084106276440764, 41.63779006702063867 ) ) ;
#19222 = AXIS2_PLACEMENT_3D ( 'NONE', #1917, #11726, #19399 ) ;
#19223 = ORIENTED_EDGE ( 'NONE', *, *, #3835, .F. ) ;
#19224 = CARTESIAN_POINT ( 'NONE',  ( 38.01140435219952707, 68.63445800887258486, 32.58608133808903773 ) ) ;
#19225 = DIRECTION ( 'NONE',  ( 0.000000000000000000, 0.000000000000000000, 1.000000000000000000 ) ) ;
#19226 = CARTESIAN_POINT ( 'NONE',  ( 38.58424406990786082, 135.3797705074273381, 34.21067981925357060 ) ) ;
#19227 = CARTESIAN_POINT ( 'NONE',  ( 30.56769828357572294, 94.69056354510921381, 8.922930725513751327 ) ) ;
#19228 = ORIENTED_EDGE ( 'NONE', *, *, #6178, .T. ) ;
#19229 = CARTESIAN_POINT ( 'NONE',  ( 148.6725454929228079, -61.68114226949890622, -16.21320343559643717 ) ) ;
#19230 = ORIENTED_EDGE ( 'NONE', *, *, #13920, .T. ) ;
#19231 = CARTESIAN_POINT ( 'NONE',  ( 38.58424406990786082, 129.3797705074273381, 34.21067981925357060 ) ) ;
#19232 = CARTESIAN_POINT ( 'NONE',  ( 48.01140435219951996, 134.2104996726487514, 34.21067981925357060 ) ) ;
#19233 = DIRECTION ( 'NONE',  ( -1.000000000000000000, 0.000000000000000000, 0.000000000000000000 ) ) ;
#19234 = DIRECTION ( 'NONE',  ( -1.186952418100008983E-16, -0.000000000000000000, -1.000000000000000000 ) ) ;
#19235 = LINE ( 'NONE', #8893, #14142 ) ;
#19236 = AXIS2_PLACEMENT_3D ( 'NONE', #3353, #1702, #8431 ) ;
#19237 = CARTESIAN_POINT ( 'NONE',  ( 38.58424406990784661, 102.2651871740939811, 35.64915139335016647 ) ) ;
#19238 = DIRECTION ( 'NONE',  ( 0.000000000000000000, 1.000000000000000000, 0.000000000000000000 ) ) ;
#19239 = CARTESIAN_POINT ( 'NONE',  ( 46.10157429594899270, 125.6604996726487542, 29.95742577749336988 ) ) ;
#19240 = CARTESIAN_POINT ( 'NONE',  ( -141.4692556286852891, -159.0630981290892976, 49.65701158161630957 ) ) ;
#19241 = CARTESIAN_POINT ( 'NONE',  ( 43.01140435219954838, 132.5344580088725763, 39.21067981925356349 ) ) ;
#19242 = CARTESIAN_POINT ( 'NONE',  ( 44.55648932407425633, 130.8844580088725706, 29.45539723777780239 ) ) ;
#19243 = CARTESIAN_POINT ( 'NONE',  ( 45.74753988029933538, 113.3297705074273125, 30.44471234641811819 ) ) ;
#19244 =( BOUNDED_CURVE ( )  B_SPLINE_CURVE ( 2, ( #15883, #12694, #20862, #2234, #796, #15782, #5644, #5531, #688, #576, #17211, #7207, #13909 ),
 .UNSPECIFIED., .F., .F. ) 
 B_SPLINE_CURVE_WITH_KNOTS ( ( 3, 2, 2, 2, 2, 2, 3 ),
 ( 0.6838235294117647189, 0.6852941176470588314, 0.6882352941176470562, 0.6911764705882352811, 0.6941176470588235059, 0.6970588235294117307, 0.6985294117647058432 ),
 .UNSPECIFIED. ) 
 CURVE ( )  GEOMETRIC_REPRESENTATION_ITEM ( )  RATIONAL_B_SPLINE_CURVE ( ( 0.9755282581475768211, 0.9755282581475768211, 1.000000000000000000, 0.9510565162951535312, 1.000000000000000000, 0.9510565162951535312, 1.000000000000000000, 0.9510565162951535312, 1.000000000000000000, 0.9510565162951535312, 1.000000000000000000, 0.9755282581475768211, 0.9755282581475768211 ) ) 
 REPRESENTATION_ITEM ( '' )  );
#19245 = CARTESIAN_POINT ( 'NONE',  ( 60.26010703883354580, 142.3196469542212697, 3.652109145728902551 ) ) ;
#19246 = DIRECTION ( 'NONE',  ( -0.000000000000000000, -0.000000000000000000, 1.000000000000000000 ) ) ;
#19247 = CARTESIAN_POINT ( 'NONE',  ( 46.59305225739526435, 94.91518717409400097, 31.60846029578754468 ) ) ;
#19248 = DIRECTION ( 'NONE',  ( 0.000000000000000000, 1.000000000000000000, 0.000000000000000000 ) ) ;
#19249 = CYLINDRICAL_SURFACE ( 'NONE', #2736, 4.999999999999997335 ) ;
#19250 = CARTESIAN_POINT ( 'NONE',  ( 67.39040179371399120, 143.9404232637865562, 4.720051584306741432 ) ) ;
#19251 = CIRCLE ( 'NONE', #4817, 5.425037101889737201 ) ;
#19252 = CARTESIAN_POINT ( 'NONE',  ( 27.67177345608778793, 143.5689829720894011, 10.27550654291302479 ) ) ;
#19253 = ADVANCED_FACE ( 'NONE', ( #5386 ), #6945, .T. ) ;
#19254 = PRODUCT_DEFINITION_SHAPE ( 'NONE', 'NONE',  #21821 ) ;
#19255 = LINE ( 'NONE', #17260, #17430 ) ;
#19256 = CARTESIAN_POINT ( 'NONE',  ( 44.37947211624943833, 77.47977050742731819, 30.00020018409699318 ) ) ;
#19257 = VERTEX_POINT ( 'NONE', #18729 ) ;
#19258 = ORIENTED_EDGE ( 'NONE', *, *, #9655, .T. ) ;
#19259 = CARTESIAN_POINT ( 'NONE',  ( -143.3790856849358306, -165.3630981290893089, 55.53486410454105027 ) ) ;
#19260 = CARTESIAN_POINT ( 'NONE',  ( 44.55648932407425633, 124.6104996726487428, 38.96596240072933170 ) ) ;
#19262 = CARTESIAN_POINT ( 'NONE',  ( 50.69626032627856915, 86.62977272806217854, -5.918438612465169335 ) ) ;
#19261 = CARTESIAN_POINT ( 'NONE',  ( 38.58424406990784661, 75.26518717409399528, 35.64915139335016647 ) ) ;
#19263 = AXIS2_PLACEMENT_3D ( 'NONE', #2686, #9431, #4561 ) ;
#19264 = EDGE_CURVE ( 'NONE', #5192, #5965, #6895, .T. ) ;
#19265 = CARTESIAN_POINT ( 'NONE',  ( -159.0959885057557983, -170.1938272943107222, 44.11586579668791330 ) ) ;
#19266 = CARTESIAN_POINT ( 'NONE',  ( 77.07719282571002850, 116.5297446719512209, 12.69640610750513865 ) ) ;
#19267 = CARTESIAN_POINT ( 'NONE',  ( -159.5594255724347761, -184.2630981290893146, 55.53486410454104316 ) ) ;
#19268 = CARTESIAN_POINT ( 'NONE',  ( -120.0322075325610740, -126.9891397928655010, 30.00000000000000000 ) ) ;
#19269 = CARTESIAN_POINT ( 'NONE',  ( 2.004595370269653287, 635.3380690778678854, -23.16745088979876499 ) ) ;
#19270 = CARTESIAN_POINT ( 'NONE',  ( 40.27526882409969033, 144.8297705074273267, 37.97664729208901946 ) ) ;
#19271 = CARTESIAN_POINT ( 'NONE',  ( 72.04953363923264931, 101.6246461802091972, -1.784078408812360017 ) ) ;
#19272 = CARTESIAN_POINT ( 'NONE',  ( 46.59305225739526435, 127.3151871740940067, 36.81289934271958941 ) ) ;
#19273 = CARTESIAN_POINT ( 'NONE',  ( 46.10157429594899270, 136.7604996726487627, 38.46393386101375711 ) ) ;
#19274 = CARTESIAN_POINT ( 'NONE',  ( -160.8964159109769696, -167.0084106276440536, 52.72008163687743121 ) ) ;
#19275 = CARTESIAN_POINT ( 'NONE',  ( 151.4773229304660731, 84.89323405393692212, -19.99999999999997868 ) ) ;
#19276 = DIRECTION ( 'NONE',  ( -0.000000000000000000, -0.000000000000000000, -1.000000000000000000 ) ) ;
#19277 = CARTESIAN_POINT ( 'NONE',  ( 14.90453237821946253, 123.0362832886413855, 8.294721248935834623 ) ) ;
#19278 = FACE_OUTER_BOUND ( 'NONE', #4800, .T. ) ;
#19279 = CARTESIAN_POINT ( 'NONE',  ( 45.74753988029933538, 106.1651871740940152, 37.97664729208901946 ) ) ;
#19280 = EDGE_LOOP ( 'NONE', ( #840, #17530, #20456, #10724 ) ) ;
#19281 = VECTOR ( 'NONE', #18499, 1000.000000000000000 ) ;
#19282 = CARTESIAN_POINT ( 'NONE',  ( 46.10157429594899270, 86.66049967264872578, 29.95742577749336988 ) ) ;
#19283 = EDGE_CURVE ( 'NONE', #13772, #7609, #18989, .T. ) ;
#19284 = ORIENTED_EDGE ( 'NONE', *, *, #10557, .F. ) ;
#19285 = CARTESIAN_POINT ( 'NONE',  ( 46.10157429594899270, 93.83445800887258770, 38.46393386101376421 ) ) ;
#19286 = CARTESIAN_POINT ( 'NONE',  ( 47.43856463449118621, 151.8797705074273097, 34.21067981925357060 ) ) ;
#19287 = CARTESIAN_POINT ( 'NONE',  ( 44.55648932407425633, 151.6104996726487570, 38.96596240072933170 ) ) ;
#19289 = CARTESIAN_POINT ( 'NONE',  ( 17.19109055900979399, 108.7710072034773532, -4.291528102762561581 ) ) ;
#19288 = CARTESIAN_POINT ( 'NONE',  ( 45.74753988029933538, 107.0651871740939640, 30.44471234641811819 ) ) ;
#19290 = CARTESIAN_POINT ( 'NONE',  ( 39.92123440845004723, 63.26049967264874141, 29.95742577749337343 ) ) ;
#19292 = LINE ( 'NONE', #14536, #18137 ) ;
#19291 = CARTESIAN_POINT ( 'NONE',  ( 157.5268905834513475, 193.0332408774651185, -29.99999999999997868 ) ) ;
#19293 = SURFACE_SIDE_STYLE ('',( #16189 ) ) ;
#19294 = CARTESIAN_POINT ( 'NONE',  ( -159.5594255724347761, -187.8630981290893089, 43.77915905869157598 ) ) ;
#19295 = DIRECTION ( 'NONE',  ( 0.000000000000000000, 0.7071067811865573427, 0.7071067811865378028 ) ) ;
#19296 = CARTESIAN_POINT ( 'NONE',  ( 40.27526882409969033, 65.66518717409398675, 30.44471234641811819 ) ) ;
#19297 = CARTESIAN_POINT ( 'NONE',  ( 23.23160898551418185, 147.7622765488190453, -10.85157364460736140 ) ) ;
#19298 = LINE ( 'NONE', #19086, #16802 ) ;
#19299 = CARTESIAN_POINT ( 'NONE',  ( -157.2955611005346270, -175.4438272943107506, 57.67623309621198047 ) ) ;
#19300 = DIRECTION ( 'NONE',  ( 0.000000000000000000, 0.000000000000000000, 1.000000000000000000 ) ) ;
#19301 = EDGE_LOOP ( 'NONE', ( #15607, #12823 ) ) ;
#19302 = CARTESIAN_POINT ( 'NONE',  ( 20.67200536010596323, 145.9528555770810385, 9.049038938933962939 ) ) ;
#19303 = LINE ( 'NONE', #1552, #14079 ) ;
#19304 = CARTESIAN_POINT ( 'NONE',  ( 44.37947211624943833, 130.0151871740939953, 38.42115945441014446 ) ) ;
#19305 = ADVANCED_FACE ( 'NONE', ( #17170, #19158, #21254 ), #1077, .F. ) ;
#19306 = CARTESIAN_POINT ( 'NONE',  ( 39.42975644700377558, 93.67977050742732104, 36.81289934271958941 ) ) ;
#19307 = ORIENTED_EDGE ( 'NONE', *, *, #8508, .F. ) ;
#19308 = EDGE_LOOP ( 'NONE', ( #9238, #14202, #3942, #4383, #1716, #8833, #9364, #15008 ) ) ;
#19309 = CARTESIAN_POINT ( 'NONE',  ( 49.55020742284296631, 92.47612394764220767, 0.1565338505643876776 ) ) ;
#19310 = EDGE_LOOP ( 'NONE', ( #11462, #10664 ) ) ;
#19311 = CARTESIAN_POINT ( 'NONE',  ( 39.92123440845004723, 113.3344580088725593, 29.95742577749337343 ) ) ;
#19312 = CARTESIAN_POINT ( 'NONE',  ( 38.96631938032478359, 76.01049967264873430, 37.14960608071593384 ) ) ;
#19313 = CARTESIAN_POINT ( 'NONE',  ( 44.37947211624943833, 77.47977050742731819, 30.00020018409699318 ) ) ;
#19314 = CARTESIAN_POINT ( 'NONE',  ( 39.42975644700377558, 137.8151871740940067, 31.60846029578754468 ) ) ;
#19315 = CARTESIAN_POINT ( 'NONE',  ( 43.01140435219951286, 89.96049967264872294, 28.95336869806222779 ) ) ;
#19316 = CARTESIAN_POINT ( 'NONE',  ( 41.61242760320212852, 154.1118385459532760, 10.79173905232880237 ) ) ;
#19317 = DIRECTION ( 'NONE',  ( -0.9385982292947088190, -0.3450121214752274179, 2.040824802394967185E-16 ) ) ;
#19318 = CARTESIAN_POINT ( 'NONE',  ( -151.4692556286852891, -159.2391397928654726, 39.14238933923362396 ) ) ;
#19319 = CARTESIAN_POINT ( 'NONE',  ( 48.01140435219951996, 158.2104996726487514, 34.21067981925357060 ) ) ;
#19320 = DIRECTION ( 'NONE',  ( -0.000000000000000000, -0.000000000000000000, 1.000000000000000000 ) ) ;
#19321 = CARTESIAN_POINT ( 'NONE',  ( 47.05648932407426344, 105.9844580088725792, 37.14960608071593384 ) ) ;
#19322 = ORIENTED_EDGE ( 'NONE', *, *, #7348, .F. ) ;
#19323 = CARTESIAN_POINT ( 'NONE',  ( 39.42975644700377558, 72.67977050742730682, 36.81289934271958941 ) ) ;
#19324 = CARTESIAN_POINT ( 'NONE',  ( -143.8425227516148084, -168.6938272943107222, 55.19815736654470584 ) ) ;
#19325 = CARTESIAN_POINT ( 'NONE',  ( 75.10802748102119608, 108.0013139708956800, -8.018167963582932600 ) ) ;
#19326 = DIRECTION ( 'NONE',  ( 0.000000000000000000, 1.000000000000000000, 0.000000000000000000 ) ) ;
#19327 = ORIENTED_EDGE ( 'NONE', *, *, #17399, .F. ) ;
#19328 = DIRECTION ( 'NONE',  ( -0.9385982292947087080, -0.3450121214752278620, 2.040824802394967678E-16 ) ) ;
#19329 = CIRCLE ( 'NONE', #10203, 10.00000000000000888 ) ;
#19330 = CARTESIAN_POINT ( 'NONE',  ( 43.01140435219951286, 125.0344580088725905, 29.21067981925356705 ) ) ;
#19331 = CARTESIAN_POINT ( 'NONE',  ( 39.42975644700377558, 138.0797705074273267, 31.60846029578754468 ) ) ;
#19332 = VERTEX_POINT ( 'NONE', #19478 ) ;
#19333 = CARTESIAN_POINT ( 'NONE',  ( 173.3794444120442506, -37.13255853780189852, 30.00000000000000000 ) ) ;
#19334 = VERTEX_POINT ( 'NONE', #17707 ) ;
#19335 = CARTESIAN_POINT ( 'NONE',  ( 46.59305225739526435, 130.5797705074273267, 36.81289934271958941 ) ) ;
#19336 = CARTESIAN_POINT ( 'NONE',  ( 47.05648932407426344, 110.5104996726487343, 31.27175355779120025 ) ) ;
#19337 = CARTESIAN_POINT ( 'NONE',  ( 43.01140435219951996, 10.71049967264875491, 29.21067981925357060 ) ) ;
#19338 = LINE ( 'NONE', #21004, #20842 ) ;
#19339 = CARTESIAN_POINT ( 'NONE',  ( 33.01140435219951286, 119.9070776186055838, 8.284271247461942878 ) ) ;
#19340 = CARTESIAN_POINT ( 'NONE',  ( -141.4692556286852891, -186.9891397928654726, 49.65701158161630957 ) ) ;
#19341 = CARTESIAN_POINT ( 'NONE',  ( 46.10157429594899270, 74.66049967264873999, 29.95742577749336988 ) ) ;
#19342 = CARTESIAN_POINT ( 'NONE',  ( -47.86331837773882825, 0.000000000000000000, -19.99999999999997513 ) ) ;
#19343 = CARTESIAN_POINT ( 'NONE',  ( -143.3790856849358306, -161.7630981290893146, 43.77915905869157598 ) ) ;
#19344 = ADVANCED_FACE ( 'NONE', ( #1182 ), #4058, .T. ) ;
#19345 = EDGE_CURVE ( 'NONE', #11274, #16314, #15947, .T. ) ;
#19346 = CARTESIAN_POINT ( 'NONE',  ( 48.01140435219951996, 109.1344580088725849, 35.83527830041809636 ) ) ;
#19347 = CARTESIAN_POINT ( 'NONE',  ( 39.92123440845004723, 134.3344580088725877, 29.95742577749337343 ) ) ;
#19348 = CARTESIAN_POINT ( 'NONE',  ( 43.01140435219951286, 112.1297705074272812, 38.86567161673127657 ) ) ;
#19349 = CARTESIAN_POINT ( 'NONE',  ( 70.95506224315714405, 115.5552942049593668, 4.842541188697900623 ) ) ;
#19350 = CARTESIAN_POINT ( 'NONE',  ( -151.4692556286852891, -188.6438272943107393, 39.74470866294723947 ) ) ;
#19351 = CARTESIAN_POINT ( 'NONE',  ( 44.37947211624943833, 98.21518717409399812, 30.00020018409699318 ) ) ;
#19352 = CARTESIAN_POINT ( 'NONE',  ( 42.21948215057684450, 91.38361825032848174, 39.21067981925355639 ) ) ;
#19353 = ORIENTED_EDGE ( 'NONE', *, *, #6350, .T. ) ;
#19354 = CARTESIAN_POINT ( 'NONE',  ( 43.01140435219951286, 75.53445800887257633, 39.21067981925356349 ) ) ;
#19355 = CARTESIAN_POINT ( 'NONE',  ( 58.57487293839693621, 150.3975950434478648, 4.362879525569486994 ) ) ;
#19356 = CARTESIAN_POINT ( 'NONE',  ( 64.38652456388278722, 138.1782414180340197, -15.12506982898978158 ) ) ;
#19357 = DIRECTION ( 'NONE',  ( 0.000000000000000000, 0.000000000000000000, -1.000000000000000000 ) ) ;
#19358 = PRODUCT_DEFINITION_FORMATION_WITH_SPECIFIED_SOURCE ( 'ANY', '', #8687, .NOT_KNOWN. ) ;
#19359 = CARTESIAN_POINT ( 'NONE',  ( 43.01140435219951286, 77.62977050742730967, 29.55568802177586107 ) ) ;
#19360 = ORIENTED_EDGE ( 'NONE', *, *, #9116, .T. ) ;
#19361 = VERTEX_POINT ( 'NONE', #7594 ) ;
#19362 = CARTESIAN_POINT ( 'NONE',  ( 41.64333658814960870, 158.7797705074273438, 30.00020018409699318 ) ) ;
#19363 = CARTESIAN_POINT ( 'NONE',  ( 131.4397495910615135, 111.2323268066561894, 4.000000000000021316 ) ) ;
#19364 = CARTESIAN_POINT ( 'NONE',  ( 43.01140435219951286, 118.4604996726487514, 39.46799094044489209 ) ) ;
#19366 = CARTESIAN_POINT ( 'NONE',  ( 74.70172802024292480, 107.1710682803345662, -6.989838304517381751 ) ) ;
#19365 = CARTESIAN_POINT ( 'NONE',  ( 40.27526882409969033, 81.56518717409399244, 37.97664729208901946 ) ) ;
#19367 =( BOUNDED_CURVE ( )  B_SPLINE_CURVE ( 2, ( #9818, #5176, #14867, #21613, #6503, #11895, #18624, #10254, #4845, #8162, #13117, #8598, #211 ),
 .UNSPECIFIED., .F., .F. ) 
 B_SPLINE_CURVE_WITH_KNOTS ( ( 3, 2, 2, 2, 2, 2, 3 ),
 ( 0.2321428571428571508, 0.2357142857142857095, 0.2428571428571428548, 0.2500000000000000000, 0.2571428571428571175, 0.2642857142857142905, 0.2678571428571428492 ),
 .UNSPECIFIED. ) 
 CURVE ( )  GEOMETRIC_REPRESENTATION_ITEM ( )  RATIONAL_B_SPLINE_CURVE ( ( 0.9755282581475767101, 0.9755282581475768211, 1.000000000000000000, 0.9510565162951535312, 1.000000000000000000, 0.9510565162951535312, 1.000000000000000000, 0.9510565162951535312, 1.000000000000000000, 0.9510565162951535312, 1.000000000000000000, 0.9755282581475768211, 0.9755282581475768211 ) ) 
 REPRESENTATION_ITEM ( '' )  );
#19368 = CARTESIAN_POINT ( 'NONE',  ( -160.8964159109769696, -172.7438272943107336, 52.72008163687743121 ) ) ;
#19369 = CARTESIAN_POINT ( 'NONE',  ( 47.05648932407426344, 112.9104996726487400, 37.14960608071593384 ) ) ;
#19370 = CARTESIAN_POINT ( 'NONE',  ( -159.5594255724347761, -187.2630981290893146, 55.53486410454104316 ) ) ;
#19371 =( NAMED_UNIT ( * ) SI_UNIT ( $, .STERADIAN. ) SOLID_ANGLE_UNIT ( ) );
#19372 = ADVANCED_FACE ( 'NONE', ( #17813 ), #15840, .F. ) ;
#19373 = CARTESIAN_POINT ( 'NONE',  ( 43.01140435219951286, 103.4604996726487371, 39.21067981925356349 ) ) ;
#19374 = CARTESIAN_POINT ( 'NONE',  ( -141.4692556286852891, -162.9891397928654726, 49.65701158161630957 ) ) ;
#19375 = CARTESIAN_POINT ( 'NONE',  ( 46.59305225739526435, 146.1797705074273495, 31.60846029578754468 ) ) ;
#19376 = CARTESIAN_POINT ( 'NONE',  ( 17.69433683334896656, 96.74512228834443306, 7.263443568815639573 ) ) ;
#19377 = CARTESIAN_POINT ( 'NONE',  ( 41.64333658814960870, 122.5151871740940095, 30.00020018409699318 ) ) ;
#19378 = CARTESIAN_POINT ( 'NONE',  ( -154.3824083646099439, -157.5584106276440650, 58.62277379824867296 ) ) ;
#19379 = CARTESIAN_POINT ( 'NONE',  ( -154.5594255724347761, -163.8891397928654499, 59.16757674456785310 ) ) ;
#19380 = CARTESIAN_POINT ( 'NONE',  ( -155.5590455049452316, -156.0406172220664303, 40.47124262348441448 ) ) ;
#19381 = CARTESIAN_POINT ( 'NONE',  ( 40.78231060393920870, 91.71360054188218669, 6.509252002934985626 ) ) ;
#19382 = CARTESIAN_POINT ( 'NONE',  ( 43.01140435219951996, 10.71049967264875491, 34.21067981925357060 ) ) ;
#19383 = CARTESIAN_POINT ( 'NONE',  ( 47.43856463449118621, 103.6151871740940038, 34.21067981925357060 ) ) ;
#19384 = ORIENTED_EDGE ( 'NONE', *, *, #14612, .F. ) ;
#19385 = CARTESIAN_POINT ( 'NONE',  ( 84.42064422693164261, 282.0082918409407284, -4.000000000000003553 ) ) ;
#19386 = ORIENTED_EDGE ( 'NONE', *, *, #20723, .F. ) ;
#19387 = CARTESIAN_POINT ( 'NONE',  ( 47.05648932407426344, 88.58445800887257349, 31.27175355779120025 ) ) ;
#19388 = CARTESIAN_POINT ( 'NONE',  ( 42.21948215057684450, 131.1113394311928175, 29.21067981925355994 ) ) ;
#19389 = CARTESIAN_POINT ( 'NONE',  ( 38.96631938032478359, 153.4104996726487400, 31.27175355779120025 ) ) ;
#19391 = CARTESIAN_POINT ( 'NONE',  ( 14.89151287784495281, 119.8505320279099209, -10.83935810001172229 ) ) ;
#19390 = CARTESIAN_POINT ( 'NONE',  ( 38.58424406990786082, 105.1151871740940038, 34.21067981925357060 ) ) ;
#19392 = CARTESIAN_POINT ( 'NONE',  ( 43.01140435219951286, 64.46049967264873715, 39.46799094044489209 ) ) ;
#19394 = CARTESIAN_POINT ( 'NONE',  ( 48.01140435219951996, 61.13445800887256354, 35.83527830041809636 ) ) ;
#19393 = CARTESIAN_POINT ( 'NONE',  ( 46.31959713345366225, 144.6883137394385130, 37.97384977752898294 ) ) ;
#19395 =( NAMED_UNIT ( * ) PLANE_ANGLE_UNIT ( ) SI_UNIT ( $, .RADIAN. ) );
#19396 = DIRECTION ( 'NONE',  ( -1.000000000000000000, 0.000000000000000000, 0.000000000000000000 ) ) ;
#19397 = CARTESIAN_POINT ( 'NONE',  ( 46.10157429594899270, 146.6604996726487400, 29.95742577749336988 ) ) ;
#19398 = CARTESIAN_POINT ( 'NONE',  ( 38.58424406990786082, 69.11518717409400381, 34.21067981925357060 ) ) ;
#19399 = DIRECTION ( 'NONE',  ( -1.000000000000000000, 0.000000000000000000, 0.000000000000000000 ) ) ;
#19400 = DIRECTION ( 'NONE',  ( -0.8302490056034133037, -0.5573926701119628069, 0.000000000000000000 ) ) ;
#19401 = CARTESIAN_POINT ( 'NONE',  ( -148.5561028927606344, -171.9938272943107336, 58.62277379824867296 ) ) ;
#19402 = CARTESIAN_POINT ( 'NONE',  ( -143.8425227516148084, -186.9584106276440423, 55.19815736654470584 ) ) ;
#19403 = VERTEX_POINT ( 'NONE', #4369 ) ;
#19404 = CARTESIAN_POINT ( 'NONE',  ( -160.8964159109769696, -173.1584106276440593, 49.65701158161630957 ) ) ;
#19405 = CARTESIAN_POINT ( 'NONE',  ( 58.41865009756546812, 150.5677012977470781, 10.35848337793017393 ) ) ;
#19406 = VERTEX_POINT ( 'NONE', #7486 ) ;
#19407 = CARTESIAN_POINT ( 'NONE',  ( 46.59305225739526435, 136.3151871740940351, 36.81289934271958941 ) ) ;
#19408 = CARTESIAN_POINT ( 'NONE',  ( 46.59305225739526435, 94.57977050742731251, 36.81289934271958941 ) ) ;
#19409 = ORIENTED_EDGE ( 'NONE', *, *, #6927, .F. ) ;
#19410 = ORIENTED_EDGE ( 'NONE', *, *, #11365, .F. ) ;
#19411 = VECTOR ( 'NONE', #5218, 1000.000000000000000 ) ;
#19412 = CARTESIAN_POINT ( 'NONE',  ( 25.21830160582964453, 141.7844325674071229, 10.15653385063274428 ) ) ;
#19413 = EDGE_CURVE ( 'NONE', #40, #21314, #9570, .T. ) ;
#19414 = EDGE_LOOP ( 'NONE', ( #13037, #2434 ) ) ;
#19415 = CARTESIAN_POINT ( 'NONE',  ( 43.01140435219951286, 111.5344580088725763, 39.46799094044489209 ) ) ;
#19416 = CARTESIAN_POINT ( 'NONE',  ( 38.01140435219952707, 75.71049967264873715, 34.21067981925357060 ) ) ;
#19417 = CARTESIAN_POINT ( 'NONE',  ( 41.64333658814960870, 72.97977050742731819, 38.42115945441014446 ) ) ;
#19418 = CARTESIAN_POINT ( 'NONE',  ( 47.43856463449118621, 139.6151871740939896, 34.21067981925357060 ) ) ;
#19419 = CARTESIAN_POINT ( 'NONE',  ( 41.46631938032478359, 90.11049967264874283, 29.45539723777780239 ) ) ;
#19420 = CARTESIAN_POINT ( 'NONE',  ( 59.73150498404358899, 90.03452709159309109, 13.76780503130795097 ) ) ;
#19421 = CARTESIAN_POINT ( 'NONE',  ( 42.35335639509444405, 94.91365384002462235, 39.17809732472422724 ) ) ;
#19422 = CARTESIAN_POINT ( 'NONE',  ( -161.4692556286853176, -158.4891397928654726, 49.65701158161630957 ) ) ;
#19423 = CYLINDRICAL_SURFACE ( 'NONE', #10841, 10.00000000000000888 ) ;
#19424 = PLANE ( 'NONE',  #8728 ) ;
#19425 = PRODUCT_DEFINITION_SHAPE ( 'NONE', 'NONE',  #21831 ) ;
#19426 = AXIS2_PLACEMENT_3D ( 'NONE', #5209, #20102, #4991 ) ;
#19427 = CARTESIAN_POINT ( 'NONE',  ( 126.8576204525573274, -126.9891397928655010, -17.64809332337413750 ) ) ;
#19428 = VECTOR ( 'NONE', #14742, 1000.000000000000227 ) ;
#19429 = VERTEX_POINT ( 'NONE', #19373 ) ;
#19430 = CARTESIAN_POINT ( 'NONE',  ( 38.58424406990786082, 78.37977050742732388, 34.21067981925357060 ) ) ;
#19431 = CARTESIAN_POINT ( 'NONE',  ( -159.0959885057557983, -167.1938272943107222, 44.11586579668791330 ) ) ;
#19432 = CARTESIAN_POINT ( 'NONE',  ( 11.74529739132928619, 133.8467647624810581, -4.446451035385589279 ) ) ;
#19433 = CARTESIAN_POINT ( 'NONE',  ( -151.4692556286852891, -193.4084106276440593, 59.56931450028537967 ) ) ;
#19434 = AXIS2_PLACEMENT_3D ( 'NONE', #21392, #6278, #9275 ) ;
#19435 = ORIENTED_EDGE ( 'NONE', *, *, #21507, .T. ) ;
#19436 = CARTESIAN_POINT ( 'NONE',  ( -262.4284940691233601, 713.9312056531377948, 0.000000000000000000 ) ) ;
#19437 = CARTESIAN_POINT ( 'NONE',  ( 43.01140435219951996, 10.71049967264875491, 39.21067981925356349 ) ) ;
#19438 = CARTESIAN_POINT ( 'NONE',  ( 38.58424406990785371, 120.5297705074273154, 35.64915139335015937 ) ) ;
#19439 = ORIENTED_EDGE ( 'NONE', *, *, #10703, .T. ) ;
#19440 = CARTESIAN_POINT ( 'NONE',  ( 46.10157429594899270, 88.73445800887256496, 29.95742577749336988 ) ) ;
#19441 = ORIENTED_EDGE ( 'NONE', *, *, #7494, .F. ) ;
#19442 = CARTESIAN_POINT ( 'NONE',  ( 44.37947211624943833, 131.4797705074273040, 30.00020018409699318 ) ) ;
#19443 = CARTESIAN_POINT ( 'NONE',  ( 47.05648932407426344, 134.5104996726487343, 31.27175355779120025 ) ) ;
#19444 = CARTESIAN_POINT ( 'NONE',  ( 39.92123440845004723, 60.23445800887256496, 38.46393386101376421 ) ) ;
#19445 = EDGE_CURVE ( 'NONE', #18846, #17048, #1565, .T. ) ;
#19446 = CARTESIAN_POINT ( 'NONE',  ( 41.46631938032478359, 111.3844580088725849, 38.96596240072933170 ) ) ;
#19447 = DIRECTION ( 'NONE',  ( 1.000000000000000000, 0.000000000000000000, 0.000000000000000000 ) ) ;
#19448 = SURFACE_STYLE_USAGE ( .BOTH. , #6329 ) ;
#19449 = CARTESIAN_POINT ( 'NONE',  ( -148.3790856849358306, -187.5891397928654953, 59.16757674456786020 ) ) ;
#19450 = EDGE_CURVE ( 'NONE', #10912, #16002, #12432, .T. ) ;
#19451 = CARTESIAN_POINT ( 'NONE',  ( 38.01140435219952707, 66.56049967264871725, 32.58608133808903773 ) ) ;
#19452 = CARTESIAN_POINT ( 'NONE',  ( 136.0872141950132175, 182.3066604549029819, 24.06090893781343709 ) ) ;
#19453 = CARTESIAN_POINT ( 'NONE',  ( -161.4692556286852607, -163.4130981290892635, 52.90620854394536821 ) ) ;
#19454 = APPLICATION_PROTOCOL_DEFINITION ( 'draft international standard', 'automotive_design', 1998, #21405 ) ;
#19455 = CARTESIAN_POINT ( 'NONE',  ( 41.46631938032478359, 131.1844580088725820, 29.45539723777780239 ) ) ;
#19456 = CARTESIAN_POINT ( 'NONE',  ( 44.37947211624943833, 101.4797705074273182, 30.00020018409699318 ) ) ;
#19457 = CARTESIAN_POINT ( 'NONE',  ( 70.86003890729777766, 114.9808142912368254, 11.86642341732858874 ) ) ;
#19458 = CARTESIAN_POINT ( 'NONE',  ( -143.8425227516148084, -192.6938272943107222, 55.19815736654470584 ) ) ;
#19459 = CARTESIAN_POINT ( 'NONE',  ( 47.43856463449118621, 94.61518717409400381, 34.21067981925357060 ) ) ;
#19460 = CARTESIAN_POINT ( 'NONE',  ( 67.34521997529867576, 314.8592298662555322, 4.000000000000003553 ) ) ;
#19461 = EDGE_LOOP ( 'NONE', ( #2356, #19884, #7149, #11798 ) ) ;
#19462 = LINE ( 'NONE', #11403, #13301 ) ;
#19463 = CARTESIAN_POINT ( 'NONE',  ( 35.69068542950036260, 86.46542255174357194, 7.577194441455407770 ) ) ;
#19464 = CARTESIAN_POINT ( 'NONE',  ( 43.96673757894181023, 91.80305570246190427, -12.62481348914368873 ) ) ;
#19465 = CARTESIAN_POINT ( 'NONE',  ( 55.11952973528949684, 87.88698225678692211, -7.065691903092018222 ) ) ;
#19466 = CARTESIAN_POINT ( 'NONE',  ( 40.27526882409969744, 74.92977050742732104, 30.44471234641812174 ) ) ;
#19467 = ORIENTED_EDGE ( 'NONE', *, *, #15712, .T. ) ;
#19468 = ORIENTED_EDGE ( 'NONE', *, *, #8443, .T. ) ;
#19469 = CARTESIAN_POINT ( 'NONE',  ( 47.43856463449118621, 151.8797705074273097, 34.21067981925357060 ) ) ;
#19470 = FACE_OUTER_BOUND ( 'NONE', #18356, .T. ) ;
#19471 = CARTESIAN_POINT ( 'NONE',  ( 38.01140435219951996, 117.8604996726487428, 35.83527830041810347 ) ) ;
#19473 = CARTESIAN_POINT ( 'NONE',  ( 13.29607544193514990, 103.0715419909171970, -4.489867183945484896 ) ) ;
#19472 = CARTESIAN_POINT ( 'NONE',  ( 45.74753988029933538, 77.06518717409399244, 30.44471234641811819 ) ) ;
#19474 = CARTESIAN_POINT ( 'NONE',  ( -151.4692556286852891, -169.1438272943107108, 59.56931450028537256 ) ) ;
#19475 = CARTESIAN_POINT ( 'NONE',  ( 34.41316853928974950, 153.0433231119815503, 10.55326060710041958 ) ) ;
#19476 = CARTESIAN_POINT ( 'NONE',  ( -148.3790856849358306, -191.4630981290893317, 40.14644641866477315 ) ) ;
#19477 =( NAMED_UNIT ( * ) SI_UNIT ( $, .STERADIAN. ) SOLID_ANGLE_UNIT ( ) );
#19478 = CARTESIAN_POINT ( 'NONE',  ( 43.01140435219951286, 80.03445800887257633, 29.21067981925356705 ) ) ;
#19479 = CARTESIAN_POINT ( 'NONE',  ( -143.3790856849358306, -162.6891397928654897, 43.77915905869157598 ) ) ;
#19480 = CARTESIAN_POINT ( 'NONE',  ( 47.43856463449117200, 136.7297705074272756, 35.64915139335016647 ) ) ;
#19481 = CARTESIAN_POINT ( 'NONE',  ( 77.21761637129371536, 122.6259224659223861, -2.498659462202352799 ) ) ;
#19482 = CARTESIAN_POINT ( 'NONE',  ( 46.59305225739526435, 121.9151871740940010, 31.60846029578754468 ) ) ;
#19483 = CARTESIAN_POINT ( 'NONE',  ( 185.6125732647967368, 204.7716666330005921, 23.27362312593913174 ) ) ;
#19484 = CARTESIAN_POINT ( 'NONE',  ( -156.1828684652451784, -155.6591478762521206, 41.49287016839741682 ) ) ;
#19485 = CARTESIAN_POINT ( 'NONE',  ( 43.01140435219951996, 119.9070776186055838, -19.99999999999998579 ) ) ;
#19486 = CARTESIAN_POINT ( 'NONE',  ( 39.92123440845005433, 135.2604996726487343, 29.95742577749336988 ) ) ;
#19487 = CARTESIAN_POINT ( 'NONE',  ( 18.01452421378985136, 106.6802099491036273, 21.62814552769798837 ) ) ;
#19488 = DIRECTION ( 'NONE',  ( 0.000000000000000000, 0.000000000000000000, 1.000000000000000000 ) ) ;
#19489 = CARTESIAN_POINT ( 'NONE',  ( 44.37947211624943833, 106.0151871740939953, 38.42115945441014446 ) ) ;
#19490 = ORIENTED_EDGE ( 'NONE', *, *, #16914, .T. ) ;
#19491 = DIRECTION ( 'NONE',  ( -0.000000000000000000, -0.000000000000000000, 1.000000000000000000 ) ) ;
#19492 = ORIENTED_EDGE ( 'NONE', *, *, #5294, .T. ) ;
#19493 =( BOUNDED_CURVE ( )  B_SPLINE_CURVE ( 2, ( #2965, #21385, #6618, #13217, #3302, #6733, #8269, #3192, #1647, #7939, #14643, #13113, #13438 ),
 .UNSPECIFIED., .F., .F. ) 
 B_SPLINE_CURVE_WITH_KNOTS ( ( 3, 2, 2, 2, 2, 2, 3 ),
 ( 0.8602941176470588758, 0.8617647058823529882, 0.8647058823529412130, 0.8676470588235294379, 0.8705882352941176627, 0.8735294117647058876, 0.8750000000000000000 ),
 .UNSPECIFIED. ) 
 CURVE ( )  GEOMETRIC_REPRESENTATION_ITEM ( )  RATIONAL_B_SPLINE_CURVE ( ( 0.9755282581475768211, 0.9755282581475777093, 1.000000000000000000, 0.9510565162951535312, 1.000000000000000000, 0.9510565162951535312, 1.000000000000000000, 0.9510565162951535312, 1.000000000000000000, 0.9510565162951535312, 1.000000000000000000, 0.9755282581475768211, 0.9755282581475768211 ) ) 
 REPRESENTATION_ITEM ( '' )  );
#19494 = CARTESIAN_POINT ( 'NONE',  ( 46.10157429594899270, 94.73445800887257917, 29.95742577749337343 ) ) ;
#19495 = CARTESIAN_POINT ( 'NONE',  ( 46.10157429594899270, 103.7344580088725792, 29.95742577749336988 ) ) ;
#19496 = CARTESIAN_POINT ( 'NONE',  ( 38.01140435219951996, 147.8604996726487570, 35.83527830041810347 ) ) ;
#19498 = CARTESIAN_POINT ( 'NONE',  ( 40.36503175183082703, 91.91162403226272204, -5.481956346182379924 ) ) ;
#19497 = CARTESIAN_POINT ( 'NONE',  ( 39.42975644700377558, 104.8151871740939924, 31.60846029578754468 ) ) ;
#19499 = CARTESIAN_POINT ( 'NONE',  ( 38.96631938032478359, 64.01049967264873430, 37.14960608071593384 ) ) ;
#19501 = DIRECTION ( 'NONE',  ( 0.000000000000000000, 0.000000000000000000, 1.000000000000000000 ) ) ;
#19500 = CARTESIAN_POINT ( 'NONE',  ( 47.75437220321179410, 144.4533750968706158, 32.59446367923829513 ) ) ;
#19502 = CARTESIAN_POINT ( 'NONE',  ( 44.55648932407425633, 118.8844580088725849, 29.45539723777780239 ) ) ;
#19503 = CARTESIAN_POINT ( 'NONE',  ( 147.5268905834513475, 193.0332408774651185, 272.0939500981630204 ) ) ;
#19504 = CARTESIAN_POINT ( 'NONE',  ( 43.01140435219951286, 72.86518717409400381, 38.86567161673127657 ) ) ;
#19505 = CARTESIAN_POINT ( 'NONE',  ( 60.49690154327523572, 149.3382625450468311, -9.565656633516235630 ) ) ;
#19506 = VECTOR ( 'NONE', #10276, 1000.000000000000000 ) ;
#19507 = DIRECTION ( 'NONE',  ( 0.000000000000000000, 0.000000000000000000, 1.000000000000000000 ) ) ;
#19508 = CARTESIAN_POINT ( 'NONE',  ( -151.4692556286852891, -173.6438272943107108, 39.74470866294723947 ) ) ;
#19509 = CARTESIAN_POINT ( 'NONE',  ( -145.6429501568359797, -184.1084106276440480, 57.67623309621197336 ) ) ;
#19510 = ORIENTED_EDGE ( 'NONE', *, *, #14991, .F. ) ;
#19511 = AXIS2_PLACEMENT_3D ( 'NONE', #1864, #3420, #10142 ) ;
#19512 = CARTESIAN_POINT ( 'NONE',  ( -151.4692556286852891, -167.9084106276440309, 39.74470866294723947 ) ) ;
#19513 = CARTESIAN_POINT ( 'NONE',  ( 70.19659433329162823, 140.8466096914638399, 17.85851290171837746 ) ) ;
#19514 = CYLINDRICAL_SURFACE ( 'NONE', #3885, 4.999999999999997335 ) ;
#19515 = CARTESIAN_POINT ( 'NONE',  ( 41.64333658814960870, 138.7151871740940123, 38.42115945441014446 ) ) ;
#19516 = CARTESIAN_POINT ( 'NONE',  ( 47.43856463449118621, 91.87977050742732388, 34.21067981925357060 ) ) ;
#19517 = ORIENTED_EDGE ( 'NONE', *, *, #4463, .F. ) ;
#19518 = ORIENTED_EDGE ( 'NONE', *, *, #16615, .T. ) ;
#19519 = ADVANCED_FACE ( 'NONE', ( #4268 ), #10787, .F. ) ;
#19520 = FILL_AREA_STYLE_COLOUR ( '', #6420 ) ;
#19521 = ORIENTED_EDGE ( 'NONE', *, *, #3391, .T. ) ;
#19522 = CARTESIAN_POINT ( 'NONE',  ( 44.55648932407425633, 117.6844580088725820, 38.96596240072933170 ) ) ;
#19523 = AXIS2_PLACEMENT_3D ( 'NONE', #9248, #21038, #5921 ) ;
#19524 = DIRECTION ( 'NONE',  ( 0.3450121214752274179, -0.9385982292947088190, 7.395570986446985676E-32 ) ) ;
#19525 = CARTESIAN_POINT ( 'NONE',  ( 38.58424406990784661, 72.52977050742731535, 35.64915139335016647 ) ) ;
#19526 = CARTESIAN_POINT ( 'NONE',  ( 45.74753988029933538, 136.1651871740939725, 37.97664729208901946 ) ) ;
#19527 = CARTESIAN_POINT ( 'NONE',  ( 38.96631938032478359, 96.41049967264873999, 31.27175355779120025 ) ) ;
#19528 = CARTESIAN_POINT ( 'NONE',  ( 40.36769960724004846, 95.04687716051704172, 29.96360841760569471 ) ) ;
#19529 = CARTESIAN_POINT ( 'NONE',  ( -154.5594255724347761, -156.0891397928654953, 40.14644641866476604 ) ) ;
#19530 = CARTESIAN_POINT ( 'NONE',  ( -120.0322075325610740, -136.9891397928655010, 30.00000000000000000 ) ) ;
#19531 = CARTESIAN_POINT ( 'NONE',  ( -151.4692556286852607, -184.7391397928654726, 59.65701158161632378 ) ) ;
#19532 = ORIENTED_EDGE ( 'NONE', *, *, #18390, .F. ) ;
#19533 = CARTESIAN_POINT ( 'NONE',  ( 45.74753988029933538, 76.42977050742729261, 37.97664729208901946 ) ) ;
#19534 = CARTESIAN_POINT ( 'NONE',  ( -145.6429501568359797, -156.8438272943107563, 57.67623309621198047 ) ) ;
#19535 = CARTESIAN_POINT ( 'NONE',  ( 13.69124840528610321, 102.2378096837820181, -5.517995706778950016 ) ) ;
#19536 = CARTESIAN_POINT ( 'NONE',  ( -145.6429501568359797, -184.1084106276440480, 57.67623309621198047 ) ) ;
#19537 = ORIENTED_EDGE ( 'NONE', *, *, #7908, .F. ) ;
#19538 = CARTESIAN_POINT ( 'NONE',  ( -157.6495955161842062, -161.0391397928654555, 58.16351966513671812 ) ) ;
#19539 = FACE_OUTER_BOUND ( 'NONE', #8563, .T. ) ;
#19540 = CARTESIAN_POINT ( 'NONE',  ( 45.74753988029934249, 122.3297705074273267, 30.44471234641812174 ) ) ;
#19541 = ORIENTED_EDGE ( 'NONE', *, *, #1718, .T. ) ;
#19542 = AXIS2_PLACEMENT_3D ( 'NONE', #10885, #415, #7147 ) ;
#19543 =( NAMED_UNIT ( * ) SI_UNIT ( $, .STERADIAN. ) SOLID_ANGLE_UNIT ( ) );
#19544 = ORIENTED_EDGE ( 'NONE', *, *, #19749, .F. ) ;
#19545 = CARTESIAN_POINT ( 'NONE',  ( 44.37947211624943833, 125.4797705074273182, 30.00020018409699318 ) ) ;
#19546 = CARTESIAN_POINT ( 'NONE',  ( -23.27144139456156324, -18.88988604584387332, 4.000000000000021316 ) ) ;
#19547 = CARTESIAN_POINT ( 'NONE',  ( 46.59305225739526435, 88.57977050742732672, 36.81289934271958941 ) ) ;
#19548 = CARTESIAN_POINT ( 'NONE',  ( 41.46631938032478359, 59.18445800887258201, 29.45539723777780239 ) ) ;
#19549 = DIRECTION ( 'NONE',  ( 0.000000000000000000, 1.000000000000000000, 0.000000000000000000 ) ) ;
#19550 = DIRECTION ( 'NONE',  ( -0.000000000000000000, 0.000000000000000000, -1.000000000000000000 ) ) ;
#19551 = CARTESIAN_POINT ( 'NONE',  ( 67.34521997529867576, 314.8592298662555322, -4.000000000000002665 ) ) ;
#19552 = CARTESIAN_POINT ( 'NONE',  ( -148.3790856849358306, -189.3891397928654783, 40.14644641866477315 ) ) ;
#19553 = CARTESIAN_POINT ( 'NONE',  ( -176.9699209214867608, -126.9891397928655010, 30.00000000000000000 ) ) ;
#19554 = CARTESIAN_POINT ( 'NONE',  ( 43.01140435219957681, 93.53445800887259054, 39.21067981925356349 ) ) ;
#19555 = CARTESIAN_POINT ( 'NONE',  ( -142.0420953463936087, -186.3938272943107393, 49.65701158161630957 ) ) ;
#19556 = PRODUCT_CONTEXT ( 'NONE', #6034, 'mechanical' ) ;
#19557 = CARTESIAN_POINT ( 'NONE',  ( 46.10157429594899270, 120.8344580088725593, 38.46393386101376421 ) ) ;
#19558 = CARTESIAN_POINT ( 'NONE',  ( 47.43856463449118621, 106.8797705074273239, 34.21067981925357060 ) ) ;
#19559 = CARTESIAN_POINT ( 'NONE',  ( 69.49514557983670215, 129.8286863358667347, 11.27102936561352742 ) ) ;
#19560 = CARTESIAN_POINT ( 'NONE',  ( -148.5561028927606344, -182.7938272943107449, 40.69124936498395328 ) ) ;
#19561 = CARTESIAN_POINT ( 'NONE',  ( 41.64333658814960870, 96.71518717409399812, 38.42115945441014446 ) ) ;
#19562 = CARTESIAN_POINT ( 'NONE',  ( -149.8854112254399240, -161.3899795514095388, 39.65701158161629536 ) ) ;
#19563 = EDGE_LOOP ( 'NONE', ( #12583, #16368, #20317, #27, #20997, #19570, #12880, #10423 ) ) ;
#19564 = FACE_BOUND ( 'NONE', #15051, .T. ) ;
#19565 = VECTOR ( 'NONE', #19326, 1000.000000000000000 ) ;
#19566 = ADVANCED_FACE ( 'NONE', ( #14514, #12864, #19585 ), #16053, .F. ) ;
#19567 = CARTESIAN_POINT ( 'NONE',  ( 29.43094928344231320, 88.48265962617873015, 0.7917390523231137012 ) ) ;
#19568 = CARTESIAN_POINT ( 'NONE',  ( 62.76710561173204894, 139.9178416638646638, -8.219927273936241008 ) ) ;
#19569 = CARTESIAN_POINT ( 'NONE',  ( 45.74753988029934249, 67.42977050742730682, 37.97664729208901235 ) ) ;
#19570 = ORIENTED_EDGE ( 'NONE', *, *, #19577, .T. ) ;
#19571 = EDGE_CURVE ( 'NONE', #20969, #9506, #21142, .T. ) ;
#19572 = VERTEX_POINT ( 'NONE', #12540 ) ;
#19573 = CARTESIAN_POINT ( 'NONE',  ( 47.43856463449117200, 157.7297705074273040, 35.64915139335016647 ) ) ;
#19574 = AXIS2_PLACEMENT_3D ( 'NONE', #2674, #12712, #4329 ) ;
#19575 = VECTOR ( 'NONE', #5967, 1000.000000000000000 ) ;
#19576 = CARTESIAN_POINT ( 'NONE',  ( -161.4692556286852891, -193.7130981290893317, 46.40781461928724383 ) ) ;
#19577 = EDGE_CURVE ( 'NONE', #5667, #735, #2507, .T. ) ;
#19578 = CARTESIAN_POINT ( 'NONE',  ( 38.96631938032478359, 117.4104996726487400, 31.27175355779120025 ) ) ;
#19579 = CARTESIAN_POINT ( 'NONE',  ( 23.63511980923729183, 148.0372221624750466, 11.16864677238829984 ) ) ;
#19580 = CARTESIAN_POINT ( 'NONE',  ( 38.01140435219952707, 65.63445800887257064, 32.58608133808903773 ) ) ;
#19581 = CARTESIAN_POINT ( 'NONE',  ( -151.4692556286852891, -170.6438272943107393, 39.74470866294723947 ) ) ;
#19582 = CARTESIAN_POINT ( 'NONE',  ( 147.8787791192428074, -126.9891397928655010, 0.3429884183836981459 ) ) ;
#19583 = CARTESIAN_POINT ( 'NONE',  ( -141.4692556286852891, -177.0630981290893260, 49.65701158161630957 ) ) ;
#19584 = SHAPE_REPRESENTATION_RELATIONSHIP ( 'NONE' , 'NONE' ,  #17468, #586 ) ;
#19585 = FACE_OUTER_BOUND ( 'NONE', #3667, .T. ) ;
#19586 = CARTESIAN_POINT ( 'NONE',  ( -148.3790856849358306, -163.5891397928654669, 59.16757674456786020 ) ) ;
#19587 = CARTESIAN_POINT ( 'NONE',  ( 39.42975644700377558, 132.6797705074273210, 36.81289934271958941 ) ) ;
#19588 = CARTESIAN_POINT ( 'NONE',  ( 26.06094713673110164, 149.7432261477326563, 2.263147435255992601 ) ) ;
#19589 = CARTESIAN_POINT ( 'NONE',  ( 47.43856463449117911, 127.7651871740940237, 32.77220824515697473 ) ) ;
#19590 = FACE_OUTER_BOUND ( 'NONE', #19301, .T. ) ;
#19591 = CARTESIAN_POINT ( 'NONE',  ( -148.5561028927606344, -159.0584106276440650, 40.69124936498395328 ) ) ;
#19592 = EDGE_CURVE ( 'NONE', #602, #19334, #5779, .T. ) ;
#19593 = CARTESIAN_POINT ( 'NONE',  ( 43.01140435219953417, 141.5344580088726048, 39.21067981925356349 ) ) ;
#19594 = VECTOR ( 'NONE', #9102, 1000.000000000000341 ) ;
#19595 = CARTESIAN_POINT ( 'NONE',  ( 48.01140435219951996, 149.3604996726487286, 32.58608133808903773 ) ) ;
#19596 = CARTESIAN_POINT ( 'NONE',  ( 29.27949416537561333, 144.5119445999418986, 23.32977622066093204 ) ) ;
#19597 = DIRECTION ( 'NONE',  ( -1.000000000000000000, 0.000000000000000000, 0.000000000000000000 ) ) ;
#19598 = CARTESIAN_POINT ( 'NONE',  ( 41.64333658814960870, 104.5151871740939953, 30.00020018409699318 ) ) ;
#19599 = EDGE_CURVE ( 'NONE', #17523, #12901, #10996, .T. ) ;
#19600 = ORIENTED_EDGE ( 'NONE', *, *, #13389, .T. ) ;
#19601 = CARTESIAN_POINT ( 'NONE',  ( 48.01140435219951996, 86.36049967264872862, 32.58608133808903773 ) ) ;
#19602 = ORIENTED_EDGE ( 'NONE', *, *, #11233, .F. ) ;
#19603 = CARTESIAN_POINT ( 'NONE',  ( 38.01140435219951996, 83.63445800887258486, 32.58608133808903773 ) ) ;
#19604 = DIRECTION ( 'NONE',  ( -1.000000000000000000, 0.000000000000000000, 0.000000000000000000 ) ) ;
#19605 = CIRCLE ( 'NONE', #12558, 10.00000000000000888 ) ;
#19606 = CARTESIAN_POINT ( 'NONE',  ( 48.01140435219951996, 149.0604996726487173, 35.83527830041810347 ) ) ;
#19608 = CARTESIAN_POINT ( 'NONE',  ( 16.96697132366095673, 109.3049078165896901, 2.732358569689224748 ) ) ;
#19607 = CARTESIAN_POINT ( 'NONE',  ( 41.64333658814960870, 105.7151871740940123, 38.42115945441014446 ) ) ;
#19609 = CARTESIAN_POINT ( 'NONE',  ( 46.10157429594899270, 62.66049967264872578, 29.95742577749337343 ) ) ;
#19611 = CARTESIAN_POINT ( 'NONE',  ( -141.4692556286852891, -182.9130981290893203, 46.40781461928724383 ) ) ;
#19610 = CARTESIAN_POINT ( 'NONE',  ( 47.85221094865248403, 144.4340178052514716, 35.50423386912935086 ) ) ;
#19612 = CARTESIAN_POINT ( 'NONE',  ( 48.01140435219951996, 118.4344580088725962, 32.58608133808903773 ) ) ;
#19613 = CARTESIAN_POINT ( 'NONE',  ( 173.3794444120442506, -126.9891397928655010, -17.64809332337413750 ) ) ;
#19614 = CARTESIAN_POINT ( 'NONE',  ( 84.42064422693164261, 282.0082918409407284, 4.000000000000003553 ) ) ;
#19615 = CARTESIAN_POINT ( 'NONE',  ( 45.22505347682923826, 59.11591767009502263, 30.37668637662395099 ) ) ;
#19616 = CARTESIAN_POINT ( 'NONE',  ( 50.33192209904863290, 153.3481575868430014, -9.922832680162505525 ) ) ;
#19617 = CARTESIAN_POINT ( 'NONE',  ( 47.43856463449117911, 151.7651871740939953, 32.77220824515697473 ) ) ;
#19618 = VECTOR ( 'NONE', #11594, 1000.000000000000227 ) ;
#19619 = DIRECTION ( 'NONE',  ( -0.000000000000000000, -0.000000000000000000, -1.000000000000000000 ) ) ;
#19620 = CARTESIAN_POINT ( 'NONE',  ( -151.4692556286852891, -175.1438272943107393, 59.56931450028537967 ) ) ;
#19621 = CARTESIAN_POINT ( 'NONE',  ( -148.5561028927606344, -183.0584106276440650, 40.69124936498395328 ) ) ;
#19622 = EDGE_CURVE ( 'NONE', #18715, #5848, #17752, .T. ) ;
#19623 = ORIENTED_EDGE ( 'NONE', *, *, #2011, .T. ) ;
#19624 = CARTESIAN_POINT ( 'NONE',  ( 39.42975644700377558, 69.41518717409400097, 36.81289934271958941 ) ) ;
#19625 = CARTESIAN_POINT ( 'NONE',  ( -148.5561028927606344, -166.2584106276440536, 58.62277379824867296 ) ) ;
#19626 = CARTESIAN_POINT ( 'NONE',  ( 57.37541587618559191, 88.74458412249896355, 12.85860293144399513 ) ) ;
#19627 = AXIS2_PLACEMENT_3D ( 'NONE', #11434, #11655, #3066 ) ;
#19628 = CARTESIAN_POINT ( 'NONE',  ( 48.01140435219951996, 112.2844580088725763, 34.21067981925357060 ) ) ;
#19629 = CARTESIAN_POINT ( 'NONE',  ( 40.27526882409969033, 137.6651871740940294, 30.44471234641811819 ) ) ;
#19630 = CARTESIAN_POINT ( 'NONE',  ( 36.78388215320455856, 153.4884242111695301, -9.370659782632428048 ) ) ;
#19631 =( BOUNDED_CURVE ( )  B_SPLINE_CURVE ( 2, ( #18060, #20071, #5067, #14644, #17949, #2966, #9706, #15089, #4726, #16406, #10031, #8157, #1206 ),
 .UNSPECIFIED., .F., .F. ) 
 B_SPLINE_CURVE_WITH_KNOTS ( ( 3, 2, 2, 2, 2, 2, 3 ),
 ( 0.5220588235294117974, 0.5235294117647059098, 0.5264705882352941346, 0.5294117647058823595, 0.5323529411764705843, 0.5352941176470588092, 0.5367647058823529216 ),
 .UNSPECIFIED. ) 
 CURVE ( )  GEOMETRIC_REPRESENTATION_ITEM ( )  RATIONAL_B_SPLINE_CURVE ( ( 0.9755282581475768211, 0.9755282581475768211, 1.000000000000000000, 0.9510565162951535312, 1.000000000000000000, 0.9510565162951535312, 1.000000000000000000, 0.9510565162951535312, 1.000000000000000000, 0.9510565162951535312, 1.000000000000000000, 0.9755282581475768211, 0.9755282581475768211 ) ) 
 REPRESENTATION_ITEM ( '' )  );
#19632 = ORIENTED_EDGE ( 'NONE', *, *, #19690, .T. ) ;
#19633 = EDGE_LOOP ( 'NONE', ( #21658, #10482, #944, #11325 ) ) ;
#19634 =( LENGTH_UNIT ( ) NAMED_UNIT ( * ) SI_UNIT ( .MILLI., .METRE. ) );
#19635 = EDGE_LOOP ( 'NONE', ( #17696, #7342, #5911, #13830 ) ) ;
#19636 = CARTESIAN_POINT ( 'NONE',  ( 47.05648932407426344, 118.5844580088725735, 31.27175355779120025 ) ) ;
#19637 = PLANE ( 'NONE',  #15377 ) ;
#19638 = AXIS2_PLACEMENT_3D ( 'NONE', #6690, #8333, #9989 ) ;
#19639 = CARTESIAN_POINT ( 'NONE',  ( 41.64333658814960870, 80.77977050742732956, 30.00020018409699318 ) ) ;
#19640 = CARTESIAN_POINT ( 'NONE',  ( 38.58424406990786082, 135.1151871740940180, 34.21067981925357060 ) ) ;
#19641 = CARTESIAN_POINT ( 'NONE',  ( 38.01140435219952707, 87.71049967264873715, 34.21067981925357060 ) ) ;
#19642 = PRESENTATION_LAYER_ASSIGNMENT (  '', '', ( #21413 ) ) ;
#19643 = CARTESIAN_POINT ( 'NONE',  ( 8.869018199820361659, 117.4101421016551967, 9.005765870029716069 ) ) ;
#19644 = CARTESIAN_POINT ( 'NONE',  ( 39.70321157094539188, 95.12584149777269715, 37.97384977752899715 ) ) ;
#19645 = CARTESIAN_POINT ( 'NONE',  ( -161.4692556286853176, -164.4891397928654726, 49.65701158161630957 ) ) ;
#19646 = CARTESIAN_POINT ( 'NONE',  ( 46.59305225739526435, 85.31518717409400665, 36.81289934271958941 ) ) ;
#19647 = ADVANCED_FACE ( 'NONE', ( #12649 ), #964, .F. ) ;
#19648 = DIRECTION ( 'NONE',  ( 1.186952418100008983E-16, 0.000000000000000000, 1.000000000000000000 ) ) ;
#19649 = CARTESIAN_POINT ( 'NONE',  ( 47.05648932407426344, 61.91049967264873288, 37.14960608071593384 ) ) ;
#19650 = ORIENTED_EDGE ( 'NONE', *, *, #8984, .T. ) ;
#19651 = CARTESIAN_POINT ( 'NONE',  ( 47.43856463449118621, 73.87977050742732388, 34.21067981925357060 ) ) ;
#19652 = CARTESIAN_POINT ( 'NONE',  ( -142.0420953463935803, -159.2438272943107620, 46.59394152635518793 ) ) ;
#19653 = CARTESIAN_POINT ( 'NONE',  ( 57.14511974427749408, 88.72838517433189054, 6.862995836283489304 ) ) ;
#19654 = CARTESIAN_POINT ( 'NONE',  ( -143.8425227516148084, -183.9584106276440707, 55.19815736654470584 ) ) ;
#19655 = VERTEX_POINT ( 'NONE', #3389 ) ;
#19656 = DIRECTION ( 'NONE',  ( 1.000000000000000000, 0.000000000000000000, 0.000000000000000000 ) ) ;
#19657 = DIRECTION ( 'NONE',  ( 0.000000000000000000, 1.000000000000000000, 0.000000000000000000 ) ) ;
#19658 = CARTESIAN_POINT ( 'NONE',  ( 44.37947211624943833, 119.4797705074273182, 30.00020018409699318 ) ) ;
#19659 = ADVANCED_FACE ( 'NONE', ( #19812 ), #19701, .T. ) ;
#19660 = VERTEX_POINT ( 'NONE', #9682 ) ;
#19661 = FILL_AREA_STYLE ('',( #12937 ) ) ;
#19662 = VERTEX_POINT ( 'NONE', #4933 ) ;
#19663 = CARTESIAN_POINT ( 'NONE',  ( 45.74753988029933538, 130.4297705074273210, 37.97664729208901946 ) ) ;
#19664 = CARTESIAN_POINT ( 'NONE',  ( 42.21948215057684450, 73.38361825032846752, 39.21067981925355639 ) ) ;
#19665 = CARTESIAN_POINT ( 'NONE',  ( 46.10157429594899270, 66.83445800887257349, 38.46393386101376421 ) ) ;
#19666 = LINE ( 'NONE', #21436, #13966 ) ;
#19667 = DIRECTION ( 'NONE',  ( 0.000000000000000000, -1.000000000000000000, 0.000000000000000000 ) ) ;
#19668 = CARTESIAN_POINT ( 'NONE',  ( 42.21948215057687293, 97.38361825032846752, 39.21067981925357060 ) ) ;
#19669 = CARTESIAN_POINT ( 'NONE',  ( -161.4692556286852607, -185.6391397928654783, 46.40781461928724383 ) ) ;
#19670 = CARTESIAN_POINT ( 'NONE',  ( 38.01140435219952707, 156.5604996726487457, 32.58608133808903773 ) ) ;
#19671 = CARTESIAN_POINT ( 'NONE',  ( 47.05648932407426344, 94.58445800887257349, 31.27175355779120025 ) ) ;
#19672 = CARTESIAN_POINT ( 'NONE',  ( -154.3824083646099439, -194.4938272943107336, 40.69124936498395328 ) ) ;
#19673 = APPLICATION_PROTOCOL_DEFINITION ( 'draft international standard', 'automotive_design', 1998, #16172 ) ;
#19674 = AXIS2_PLACEMENT_3D ( 'NONE', #2714, #17912, #16371 ) ;
#19675 = CARTESIAN_POINT ( 'NONE',  ( 39.92123440845004723, 123.2344580088725650, 38.46393386101376421 ) ) ;
#19676 = CARTESIAN_POINT ( 'NONE',  ( 40.27526882409969033, 99.82977050742729830, 37.97664729208901946 ) ) ;
#19677 = CARTESIAN_POINT ( 'NONE',  ( 65.38103680468944390, 137.2114283014329317, 17.93782343147312730 ) ) ;
#19678 = CARTESIAN_POINT ( 'NONE',  ( -154.3824083646099439, -181.2938272943107449, 58.62277379824867296 ) ) ;
#19679 = CARTESIAN_POINT ( 'NONE',  ( 47.43856463449117911, 94.46518717409399812, 35.64915139335015937 ) ) ;
#19680 = CARTESIAN_POINT ( 'NONE',  ( -143.9637021292201950, -116.9891397928655010, 62.65701158161630957 ) ) ;
#19681 = EDGE_LOOP ( 'NONE', ( #19978, #9858, #4635, #9095 ) ) ;
#19682 = DIRECTION ( 'NONE',  ( 0.000000000000000000, 0.000000000000000000, -1.000000000000000000 ) ) ;
#19683 = ADVANCED_FACE ( 'NONE', ( #16821 ), #9791, .T. ) ;
#19684 = CARTESIAN_POINT ( 'NONE',  ( 51.78234217841457365, 152.9971814535558963, 4.124977536042813142 ) ) ;
#19685 = CARTESIAN_POINT ( 'NONE',  ( 29.48178659935447854, 144.5857871963822845, 17.33364154221121467 ) ) ;
#19686 = CARTESIAN_POINT ( 'NONE',  ( 44.37947211624943833, 65.47977050742731819, 30.00020018409699318 ) ) ;
#19687 = ORIENTED_EDGE ( 'NONE', *, *, #4893, .F. ) ;
#19688 = ORIENTED_EDGE ( 'NONE', *, *, #9067, .F. ) ;
#19689 = CARTESIAN_POINT ( 'NONE',  ( 41.64333658814960870, 153.9797705074273324, 38.42115945441014446 ) ) ;
#19690 = EDGE_CURVE ( 'NONE', #5881, #4358, #18374, .T. ) ;
#19691 = VECTOR ( 'NONE', #9701, 1000.000000000000000 ) ;
#19692 = EDGE_CURVE ( 'NONE', #14823, #15585, #11420, .T. ) ;
#19693 =( BOUNDED_CURVE ( )  B_SPLINE_CURVE ( 2, ( #1549, #21726, #13344, #6510, #16961, #13230, #20081, #10153, #19967, #11572, #18301, #4968, #16639 ),
 .UNSPECIFIED., .F., .F. ) 
 B_SPLINE_CURVE_WITH_KNOTS ( ( 3, 2, 2, 2, 2, 2, 3 ),
 ( 0.7867647058823529216, 0.7882352941176470340, 0.7911764705882352589, 0.7941176470588234837, 0.7970588235294118196, 0.8000000000000000444, 0.8014705882352941568 ),
 .UNSPECIFIED. ) 
 CURVE ( )  GEOMETRIC_REPRESENTATION_ITEM ( )  RATIONAL_B_SPLINE_CURVE ( ( 0.9755282581475768211, 0.9755282581475768211, 1.000000000000000000, 0.9510565162951535312, 1.000000000000000000, 0.9510565162951535312, 1.000000000000000000, 0.9510565162951535312, 1.000000000000000000, 0.9510565162951535312, 1.000000000000000000, 0.9755282581475768211, 0.9755282581475768211 ) ) 
 REPRESENTATION_ITEM ( '' )  );
#19694 = DIRECTION ( 'NONE',  ( 0.000000000000000000, 1.000000000000000000, 0.000000000000000000 ) ) ;
#19695 = CARTESIAN_POINT ( 'NONE',  ( 38.01140435219951996, 114.8604996726487570, 35.83527830041810347 ) ) ;
#19696 = CARTESIAN_POINT ( 'NONE',  ( 38.58424406990786082, 72.11518717409400381, 34.21067981925357060 ) ) ;
#19697 = CARTESIAN_POINT ( 'NONE',  ( 42.21948215057684450, 66.45757658655229250, 39.21067981925355639 ) ) ;
#19698 = CARTESIAN_POINT ( 'NONE',  ( -160.8964159109769696, -161.0438272943107165, 46.59394152635518083 ) ) ;
#19699 = CARTESIAN_POINT ( 'NONE',  ( -141.4692556286852891, -166.1391397928654783, 52.90620854394536821 ) ) ;
#19700 = CARTESIAN_POINT ( 'NONE',  ( -159.5594255724347761, -178.2630981290893146, 55.53486410454104316 ) ) ;
#19701 = CYLINDRICAL_SURFACE ( 'NONE', #12122, 4.999999999999997335 ) ;
#19702 = CARTESIAN_POINT ( 'NONE',  ( 39.92123440845004723, 156.2344580088725934, 38.46393386101376421 ) ) ;
#19703 = CARTESIAN_POINT ( 'NONE',  ( 39.42975644700377558, 132.0797705074273267, 31.60846029578754468 ) ) ;
#19704 = CARTESIAN_POINT ( 'NONE',  ( 22.58852954093744714, 92.33198060352846426, 14.04912700239559520 ) ) ;
#19705 = CARTESIAN_POINT ( 'NONE',  ( 39.42975644700377558, 125.8151871740940067, 31.60846029578754468 ) ) ;
#19706 = CARTESIAN_POINT ( 'NONE',  ( -159.5594255724347761, -182.7891397928654840, 43.77915905869157598 ) ) ;
#19707 = CARTESIAN_POINT ( 'NONE',  ( -159.0959885057557983, -157.8584106276440480, 55.19815736654470584 ) ) ;
#19708 = LINE ( 'NONE', #9689, #20698 ) ;
#19709 = LINE ( 'NONE', #17929, #3955 ) ;
#19710 = CARTESIAN_POINT ( 'NONE',  ( 41.61464536962099459, 148.1530905165343768, 16.86614982034995691 ) ) ;
#19711 = CARTESIAN_POINT ( 'NONE',  ( -151.4692556286852891, -187.7391397928655010, 59.65701158161632378 ) ) ;
#19712 = ORIENTED_EDGE ( 'NONE', *, *, #4689, .F. ) ;
#19713 = CARTESIAN_POINT ( 'NONE',  ( 43.01140435219951286, 85.46049967264872294, 39.21067981925356349 ) ) ;
#19714 = ORIENTED_EDGE ( 'NONE', *, *, #16774, .F. ) ;
#19715 = CARTESIAN_POINT ( 'NONE',  ( 46.10157429594899270, 79.73445800887257917, 29.95742577749337343 ) ) ;
#19716 = CARTESIAN_POINT ( 'NONE',  ( 48.01140435219951996, 103.2844580088725763, 34.21067981925357060 ) ) ;
#19717 = AXIS2_PLACEMENT_3D ( 'NONE', #16596, #18373, #6917 ) ;
#19718 = CARTESIAN_POINT ( 'NONE',  ( 38.01140435219951996, 141.5604996726487457, 32.58608133808903773 ) ) ;
#19720 = CARTESIAN_POINT ( 'NONE',  ( 70.89290225163276205, 123.5572941793614206, -0.4820434552990647825 ) ) ;
#19719 = CARTESIAN_POINT ( 'NONE',  ( 47.43856463449117200, 94.76518717409398107, 32.77220824515698183 ) ) ;
#19721 = CARTESIAN_POINT ( 'NONE',  ( -151.4692556286852891, -172.4084106276440309, 59.56931450028537967 ) ) ;
#19722 = CARTESIAN_POINT ( 'NONE',  ( 39.92123440845004723, 60.26049967264872720, 29.95742577749337343 ) ) ;
#19724 = PLANE ( 'NONE',  #6199 ) ;
#19723 = DIRECTION ( 'NONE',  ( -0.000000000000000000, -0.000000000000000000, -1.000000000000000000 ) ) ;
#19725 = CARTESIAN_POINT ( 'NONE',  ( -143.3790856849358306, -189.3630981290893089, 55.53486410454105027 ) ) ;
#19726 = CARTESIAN_POINT ( 'NONE',  ( 48.01140435219951996, 79.43445800887258201, 32.58608133808903773 ) ) ;
#19727 = CARTESIAN_POINT ( 'NONE',  ( 46.10157429594899270, 115.7344580088725650, 29.95742577749336988 ) ) ;
#19728 = CARTESIAN_POINT ( 'NONE',  ( 46.59305225739526435, 61.91518717409400097, 31.60846029578754468 ) ) ;
#19729 = EDGE_CURVE ( 'NONE', #21725, #15219, #6300, .T. ) ;
#19730 = DIRECTION ( 'NONE',  ( 0.000000000000000000, -1.000000000000000000, 0.000000000000000000 ) ) ;
#19731 = DIRECTION ( 'NONE',  ( 0.000000000000000000, 0.000000000000000000, 1.000000000000000000 ) ) ;
#19732 = CARTESIAN_POINT ( 'NONE',  ( -143.8425227516148084, -168.6938272943107222, 55.19815736654470584 ) ) ;
#19733 = CARTESIAN_POINT ( 'NONE',  ( -159.0959885057557983, -188.4584106276440423, 44.11586579668791330 ) ) ;
#19734 = VERTEX_POINT ( 'NONE', #13192 ) ;
#19735 = CARTESIAN_POINT ( 'NONE',  ( 39.42975644700377558, 68.81518717409400665, 31.60846029578754468 ) ) ;
#19736 = CARTESIAN_POINT ( 'NONE',  ( -142.0420953463935803, -168.5084106276440536, 46.59394152635518793 ) ) ;
#19737 = CARTESIAN_POINT ( 'NONE',  ( 16.10574266336056226, 141.2029798434031989, 15.83487214029357659 ) ) ;
#19738 = FACE_OUTER_BOUND ( 'NONE', #7286, .T. ) ;
#19739 = CARTESIAN_POINT ( 'NONE',  ( 41.64333658814960870, 132.7151871740940123, 38.42115945441014446 ) ) ;
#19740 = AXIS2_PLACEMENT_3D ( 'NONE', #18957, #3859, #5820 ) ;
#19741 = CARTESIAN_POINT ( 'NONE',  ( 39.81857293680397447, 85.90283706545402254, -5.561266875997713299 ) ) ;
#19742 = VERTEX_POINT ( 'NONE', #11310 ) ;
#19743 = EDGE_LOOP ( 'NONE', ( #2872, #11323, #3485, #12882 ) ) ;
#19744 = CARTESIAN_POINT ( 'NONE',  ( 50.77370750611731154, 147.0167679772302165, 11.22784935402935957 ) ) ;
#19745 = EDGE_LOOP ( 'NONE', ( #19687, #8634, #14988, #1038 ) ) ;
#19746 = CARTESIAN_POINT ( 'NONE',  ( 39.92123440845004723, 110.3344580088725877, 29.95742577749337343 ) ) ;
#19747 = CARTESIAN_POINT ( 'NONE',  ( 47.05648932407426344, 116.5104996726487485, 31.27175355779120025 ) ) ;
#19748 = ADVANCED_FACE ( 'NONE', ( #13083 ), #16379, .T. ) ;
#19749 = EDGE_CURVE ( 'NONE', #14572, #14601, #18417, .T. ) ;
#19750 = CARTESIAN_POINT ( 'NONE',  ( 47.43856463449117200, 80.02977050742732956, 32.77220824515698183 ) ) ;
#19752 = CARTESIAN_POINT ( 'NONE',  ( 50.77370750611731154, 147.0167679772302165, 11.22784935402935957 ) ) ;
#19751 = CARTESIAN_POINT ( 'NONE',  ( 38.58424406990786082, 129.1151871740940180, 34.21067981925357060 ) ) ;
#19753 = CARTESIAN_POINT ( 'NONE',  ( 39.92123440845004723, 93.26049967264872009, 29.95742577749337343 ) ) ;
#19754 = CARTESIAN_POINT ( 'NONE',  ( -158.9748091281504401, -116.9891397928655010, 36.65701158161628115 ) ) ;
#19755 = CARTESIAN_POINT ( 'NONE',  ( 40.50968990821500171, 95.03214066145851291, 29.87844397536261454 ) ) ;
#19756 = CARTESIAN_POINT ( 'NONE',  ( -159.5594255724347761, -164.7891397928654555, 43.77915905869157598 ) ) ;
#19757 = CARTESIAN_POINT ( 'NONE',  ( 47.43856463449117200, 88.76518717409399528, 32.77220824515698183 ) ) ;
#19758 = CARTESIAN_POINT ( 'NONE',  ( 40.79112291011433200, 144.8101386900725061, 38.70263932541808316 ) ) ;
#19759 = DIRECTION ( 'NONE',  ( -1.140132994654635861E-16, -0.000000000000000000, -1.000000000000000000 ) ) ;
#19760 = CARTESIAN_POINT ( 'NONE',  ( 76.17254549292280785, -61.68114226949890622, 10.00000000000001599 ) ) ;
#19761 = ORIENTED_EDGE ( 'NONE', *, *, #17120, .F. ) ;
#19762 = CARTESIAN_POINT ( 'NONE',  ( 40.27526882409969033, 75.82977050742731251, 37.97664729208901946 ) ) ;
#19763 = CARTESIAN_POINT ( 'NONE',  ( -151.4692556286852891, -160.1438272943107393, 59.56931450028537967 ) ) ;
#19764 = CARTESIAN_POINT ( 'NONE',  ( 16.30372524420941716, 141.3216567370616019, 9.839263250375132941 ) ) ;
#19765 = CARTESIAN_POINT ( 'NONE',  ( -160.8964159109769696, -182.0084106276440821, 52.72008163687743121 ) ) ;
#19766 = ORIENTED_EDGE ( 'NONE', *, *, #7072, .T. ) ;
#19767 = CARTESIAN_POINT ( 'NONE',  ( -151.4692556286852607, -160.7391397928654158, 59.65701158161632378 ) ) ;
#19768 = PLANE ( 'NONE',  #771 ) ;
#19769 = CARTESIAN_POINT ( 'NONE',  ( 44.37947211624943833, 121.2797705074273296, 38.42115945441014446 ) ) ;
#19770 = VERTEX_POINT ( 'NONE', #13840 ) ;
#19771 = CARTESIAN_POINT ( 'NONE',  ( 47.05648932407426344, 88.58445800887257349, 31.27175355779120025 ) ) ;
#19772 = VERTEX_POINT ( 'NONE', #3822 ) ;
#19774 = EDGE_CURVE ( 'NONE', #4183, #2361, #17249, .T. ) ;
#19773 = CARTESIAN_POINT ( 'NONE',  ( -153.0531000319306827, -155.2362167067690280, 39.65701158161629536 ) ) ;
#19775 = ADVANCED_FACE ( 'NONE', ( #6918 ), #5146, .F. ) ;
#19776 = CARTESIAN_POINT ( 'NONE',  ( 38.96631938032478359, 66.08445800887258770, 37.14960608071593384 ) ) ;
#19777 = AXIS2_PLACEMENT_3D ( 'NONE', #14302, #21260, #6139 ) ;
#19778 = VECTOR ( 'NONE', #19657, 1000.000000000000000 ) ;
#19779 = CARTESIAN_POINT ( 'NONE',  ( 43.01140435219951996, 153.5344580088726048, 39.21067981925357060 ) ) ;
#19780 = CARTESIAN_POINT ( 'NONE',  ( 185.6125732647967368, 204.7716666330005921, 23.27362312593913174 ) ) ;
#19781 = CARTESIAN_POINT ( 'NONE',  ( 38.01140435219952707, 96.56049967264871725, 32.58608133808903773 ) ) ;
#19782 = CARTESIAN_POINT ( 'NONE',  ( -145.2889157411863721, -187.4391397928654612, 58.16351966513671812 ) ) ;
#19783 = LINE ( 'NONE', #4676, #21053 ) ;
#19784 = CARTESIAN_POINT ( 'NONE',  ( 42.21948215057684450, 102.0373810949690210, 29.21067981925356705 ) ) ;
#19785 = CARTESIAN_POINT ( 'NONE',  ( -160.8964159109769696, -188.0438272943107449, 46.59394152635518793 ) ) ;
#19786 = CONTEXT_DEPENDENT_SHAPE_REPRESENTATION ( #8178, #3263 ) ;
#19787 = VECTOR ( 'NONE', #19246, 1000.000000000000000 ) ;
#19788 = CARTESIAN_POINT ( 'NONE',  ( 39.92123440845004723, 120.2344580088725650, 38.46393386101376421 ) ) ;
#19789 = CARTESIAN_POINT ( 'NONE',  ( 38.58424406990784661, 108.2297705074273182, 32.77220824515698183 ) ) ;
#19790 = CARTESIAN_POINT ( 'NONE',  ( 71.17671054099098171, 117.3556635612232810, 18.77100214853170357 ) ) ;
#19791 = CARTESIAN_POINT ( 'NONE',  ( -142.0420953463935803, -180.2438272943107052, 46.59394152635518793 ) ) ;
#19792 = CARTESIAN_POINT ( 'NONE',  ( 45.74753988029934249, 86.06518717409402086, 30.44471234641812174 ) ) ;
#19793 = DIRECTION ( 'NONE',  ( 0.000000000000000000, 0.000000000000000000, 1.000000000000000000 ) ) ;
#19794 = ORIENTED_EDGE ( 'NONE', *, *, #6609, .T. ) ;
#19795 = DIRECTION ( 'NONE',  ( 0.000000000000000000, 0.000000000000000000, 1.000000000000000000 ) ) ;
#19796 = CARTESIAN_POINT ( 'NONE',  ( 45.29500579500201951, 154.0643053174194961, 10.91066218119221709 ) ) ;
#19797 = CARTESIAN_POINT ( 'NONE',  ( 47.43856463449117911, 145.7297705074273040, 35.64915139335015937 ) ) ;
#19798 = CARTESIAN_POINT ( 'NONE',  ( 20.44379504597808861, 136.6827000062168338, -10.12478428749056469 ) ) ;
#19799 = AXIS2_PLACEMENT_3D ( 'NONE', #17719, #17615, #6372 ) ;
#19800 = CARTESIAN_POINT ( 'NONE',  ( 46.59305225739526435, 68.17977050742732104, 31.60846029578754468 ) ) ;
#19801 = ORIENTED_EDGE ( 'NONE', *, *, #2682, .T. ) ;
#19802 = VERTEX_POINT ( 'NONE', #18704 ) ;
#19803 = CARTESIAN_POINT ( 'NONE',  ( 39.42975644700377558, 144.6797705074273495, 36.81289934271958941 ) ) ;
#19804 = EDGE_CURVE ( 'NONE', #9910, #1013, #1674, .T. ) ;
#19805 = DIRECTION ( 'NONE',  ( -0.3450121214752274734, 0.9385982292947088190, 0.000000000000000000 ) ) ;
#19806 = CARTESIAN_POINT ( 'NONE',  ( 47.05648932407426344, 106.9104996726487400, 37.14960608071593384 ) ) ;
#19807 = CARTESIAN_POINT ( 'NONE',  ( 44.37947211624943833, 65.21518717409399812, 30.00020018409699318 ) ) ;
#19808 = CARTESIAN_POINT ( 'NONE',  ( -97.23064952102208736, 13.78046159333444720, -19.99999999999997868 ) ) ;
#19809 = CARTESIAN_POINT ( 'NONE',  ( -148.5561028927606344, -164.7938272943107449, 40.69124936498395328 ) ) ;
#19810 = CARTESIAN_POINT ( 'NONE',  ( 43.01140435219951286, 156.5344580088725479, 39.21067981925355639 ) ) ;
#19811 = CARTESIAN_POINT ( 'NONE',  ( -157.6495955161842062, -176.0130981290893146, 41.15050349809590102 ) ) ;
#19812 = FACE_OUTER_BOUND ( 'NONE', #4232, .T. ) ;
#19813 = CARTESIAN_POINT ( 'NONE',  ( 48.01140435219951996, 148.4344580088725536, 32.58608133808903773 ) ) ;
#19814 = CARTESIAN_POINT ( 'NONE',  ( 39.42975644700377558, 129.0797705074273267, 31.60846029578754468 ) ) ;
#19815 = CARTESIAN_POINT ( 'NONE',  ( 34.18339000214019308, 153.0669919960894845, 16.54886172077450368 ) ) ;
#19816 = CARTESIAN_POINT ( 'NONE',  ( 40.27526882409969744, 113.6651871740939868, 30.44471234641812174 ) ) ;
#19817 = DIRECTION ( 'NONE',  ( 1.000000000000000000, 0.000000000000000000, 0.000000000000000000 ) ) ;
#19818 = CARTESIAN_POINT ( 'NONE',  ( 42.21948215057683740, 150.0373810949690210, 29.21067981925356705 ) ) ;
#19819 = LINE ( 'NONE', #18153, #9093 ) ;
#19820 = CARTESIAN_POINT ( 'NONE',  ( 47.05648932407426344, 149.5104996726487343, 31.27175355779120025 ) ) ;
#19821 = CARTESIAN_POINT ( 'NONE',  ( 57.03263806925237844, 95.34629841206742640, 19.84245794357962822 ) ) ;
#19822 =( BOUNDED_CURVE ( )  B_SPLINE_CURVE ( 2, ( #2370, #21005, #12618, #20892, #2158, #20784, #4239 ),
 .UNSPECIFIED., .F., .F. ) 
 B_SPLINE_CURVE_WITH_KNOTS ( ( 3, 2, 2, 3 ),
 ( 0.000000000000000000, 0.002941176470588235253, 0.005882352941176470507, 0.007352941176470590735 ),
 .UNSPECIFIED. ) 
 CURVE ( )  GEOMETRIC_REPRESENTATION_ITEM ( )  RATIONAL_B_SPLINE_CURVE ( ( 1.000000000000000000, 0.9510565162951535312, 1.000000000000000000, 0.9510565162951535312, 1.000000000000000000, 0.9755282581475767101, 0.9755282581475768211 ) ) 
 REPRESENTATION_ITEM ( '' )  );
#19823 = ORIENTED_EDGE ( 'NONE', *, *, #11878, .T. ) ;
#19824 = FACE_BOUND ( 'NONE', #19310, .T. ) ;
#19825 = VERTEX_POINT ( 'NONE', #11371 ) ;
#19826 = CARTESIAN_POINT ( 'NONE',  ( 48.01140435219951996, 79.13445800887258486, 35.83527830041810347 ) ) ;
#19827 = DIRECTION ( 'NONE',  ( 1.648795714028702312E-16, 6.060681657195960733E-17, 1.000000000000000000 ) ) ;
#19828 = CARTESIAN_POINT ( 'NONE',  ( 39.92123440845004723, 142.1604996726487400, 38.46393386101376421 ) ) ;
#19830 = CARTESIAN_POINT ( 'NONE',  ( 33.89447768034496278, 93.30632465966320410, 1.780072726204736000 ) ) ;
#19829 = CARTESIAN_POINT ( 'NONE',  ( 40.27526882409969033, 98.66518717409400097, 30.44471234641811819 ) ) ;
#19831 = ADVANCED_FACE ( 'NONE', ( #9115 ), #4539, .T. ) ;
#19832 = CARTESIAN_POINT ( 'NONE',  ( -154.3824083646099439, -166.5584106276440366, 58.62277379824867296 ) ) ;
#19833 = CARTESIAN_POINT ( 'NONE',  ( -145.6429501568359797, -189.8438272943106710, 57.67623309621197336 ) ) ;
#19835 = CARTESIAN_POINT ( 'NONE',  ( -176.9699209214867608, -126.9891397928655010, 67.64809332337415526 ) ) ;
#19834 = CARTESIAN_POINT ( 'NONE',  ( -157.6495955161842062, -179.0130981290892862, 41.15050349809589392 ) ) ;
#19836 = CARTESIAN_POINT ( 'NONE',  ( -176.9699209214867324, -126.9891397928655010, -72.64809332337415526 ) ) ;
#19837 = CARTESIAN_POINT ( 'NONE',  ( -149.8854112254399240, -175.6622583705452030, 59.65701158161632378 ) ) ;
#19838 = CARTESIAN_POINT ( 'NONE',  ( 38.01140435219952707, 78.56049967264873146, 32.58608133808903773 ) ) ;
#19839 = CARTESIAN_POINT ( 'NONE',  ( 45.74753988029933538, 157.4297705074273495, 37.97664729208901946 ) ) ;
#19840 = LINE ( 'NONE', #13546, #979 ) ;
#19841 = CARTESIAN_POINT ( 'NONE',  ( 61.76154402333882132, 148.5480768402654803, 4.482004293238171400 ) ) ;
#19842 = CARTESIAN_POINT ( 'NONE',  ( -154.3824083646099439, -158.4938272943107052, 40.69124936498395328 ) ) ;
#19843 = CARTESIAN_POINT ( 'NONE',  ( -154.3824083646099439, -188.7584106276440536, 40.69124936498395328 ) ) ;
#19844 = ORIENTED_EDGE ( 'NONE', *, *, #16678, .F. ) ;
#19845 = CARTESIAN_POINT ( 'NONE',  ( 38.58424406990785371, 69.26518717409399528, 35.64915139335015937 ) ) ;
#19846 = CARTESIAN_POINT ( 'NONE',  ( -145.6429501568359797, -171.2084106276440707, 41.63779006702063867 ) ) ;
#19847 = CARTESIAN_POINT ( 'NONE',  ( 46.82521527361338087, 85.80558333884177102, 13.21562623509259282 ) ) ;
#19848 = CARTESIAN_POINT ( 'NONE',  ( -136.4581486297550441, -116.9891397928655010, 49.65701158161631668 ) ) ;
#19849 = CARTESIAN_POINT ( 'NONE',  ( 38.58424406990786082, 126.1151871740940038, 34.21067981925357060 ) ) ;
#19850 = EDGE_CURVE ( 'NONE', #4977, #12281, #7353, .T. ) ;
#19851 = CARTESIAN_POINT ( 'NONE',  ( 66.98923854426821833, 144.2286169274386509, -8.299483363615854259 ) ) ;
#19852 = ORIENTED_EDGE ( 'NONE', *, *, #18492, .F. ) ;
#19853 = ORIENTED_EDGE ( 'NONE', *, *, #6437, .F. ) ;
#19854 = CIRCLE ( 'NONE', #18079, 27.14138364107347812 ) ;
#19855 = APPLICATION_CONTEXT ( 'automotive_design' ) ;
#19856 = CARTESIAN_POINT ( 'NONE',  ( 67.15412698936957270, 134.4792784496449087, 12.06138812558265805 ) ) ;
#19857 = VERTEX_POINT ( 'NONE', #14679 ) ;
#19858 = EDGE_CURVE ( 'NONE', #6015, #3147, #4035, .T. ) ;
#19859 = CARTESIAN_POINT ( 'NONE',  ( 46.10157429594899270, 108.8344580088725735, 38.46393386101376421 ) ) ;
#19860 = DIRECTION ( 'NONE',  ( -1.000000000000000000, 0.000000000000000000, 0.000000000000000000 ) ) ;
#19861 = CARTESIAN_POINT ( 'NONE',  ( 47.43856463449118621, 67.87977050742730967, 34.21067981925357060 ) ) ;
#19863 = CARTESIAN_POINT ( 'NONE',  ( 46.56541826512206228, 91.93282113015048651, 0.2755065429245392439 ) ) ;
#19862 = CARTESIAN_POINT ( 'NONE',  ( 45.74753988029933538, 130.1651871740940010, 37.97664729208901946 ) ) ;
#19864 = VECTOR ( 'NONE', #15972, 1000.000000000000114 ) ;
#19865 = EDGE_CURVE ( 'NONE', #18529, #4573, #11069, .T. ) ;
#19866 = CARTESIAN_POINT ( 'NONE',  ( 39.92123440845004723, 79.16049967264873999, 38.46393386101376421 ) ) ;
#19867 = CARTESIAN_POINT ( 'NONE',  ( 23.42018083028975184, 147.9700754799198705, 17.16443675223517573 ) ) ;
#19868 = DIRECTION ( 'NONE',  ( 0.000000000000000000, 1.000000000000000000, 0.000000000000000000 ) ) ;
#19869 = DIRECTION ( 'NONE',  ( 1.000000000000000000, 0.000000000000000000, 0.000000000000000000 ) ) ;
#19870 = CARTESIAN_POINT ( 'NONE',  ( 41.64333658814960870, 87.71518717409399812, 38.42115945441014446 ) ) ;
#19871 = CARTESIAN_POINT ( 'NONE',  ( 43.01140435219951286, 107.9604996726487229, 29.21067981925356705 ) ) ;
#19872 = CARTESIAN_POINT ( 'NONE',  ( -151.4692556286852891, -186.2391397928655010, 39.65701158161630246 ) ) ;
#19873 = ORIENTED_EDGE ( 'NONE', *, *, #13459, .F. ) ;
#19874 = CARTESIAN_POINT ( 'NONE',  ( 39.42975644700377558, 63.07977050742731251, 31.60846029578754468 ) ) ;
#19875 = CARTESIAN_POINT ( 'NONE',  ( -148.5561028927606344, -158.7938272943107449, 40.69124936498395328 ) ) ;
#19876 = CARTESIAN_POINT ( 'NONE',  ( 22.46358530849972723, 92.52609567587644790, 8.053519324161520387 ) ) ;
#19877 = CARTESIAN_POINT ( 'NONE',  ( -145.6429501568359797, -190.1084106276440195, 57.67623309621198047 ) ) ;
#19878 = ORIENTED_EDGE ( 'NONE', *, *, #13823, .T. ) ;
#19879 = EDGE_CURVE ( 'NONE', #9411, #17454, #3922, .T. ) ;
#19880 = FACE_BOUND ( 'NONE', #20634, .T. ) ;
#19881 = DIRECTION ( 'NONE',  ( -0.9609212714474144601, -0.2768218020313507610, 0.000000000000000000 ) ) ;
#19882 = CARTESIAN_POINT ( 'NONE',  ( 38.58424406990785371, 123.5297705074273438, 35.64915139335015937 ) ) ;
#19883 = CARTESIAN_POINT ( 'NONE',  ( 13.69124840528610321, 102.2378096837820181, -5.517995706778950016 ) ) ;
#19884 = ORIENTED_EDGE ( 'NONE', *, *, #7644, .T. ) ;
#19885 = EDGE_CURVE ( 'NONE', #13022, #10776, #6159, .T. ) ;
#19886 =( LENGTH_UNIT ( ) NAMED_UNIT ( * ) SI_UNIT ( .MILLI., .METRE. ) );
#19887 = EDGE_LOOP ( 'NONE', ( #4094, #21374, #1774, #13769, #17526, #14774 ) ) ;
#19888 = CARTESIAN_POINT ( 'NONE',  ( 39.42975644700377558, 117.6797705074273210, 36.81289934271958941 ) ) ;
#19889 = CARTESIAN_POINT ( 'NONE',  ( 43.01140435219957681, 71.96049967264872294, 29.21067981925356705 ) ) ;
#19890 = CARTESIAN_POINT ( 'NONE',  ( 38.58424406990784661, 87.22977050742731819, 32.77220824515698183 ) ) ;
#19891 = CARTESIAN_POINT ( 'NONE',  ( 40.27526882409969033, 158.6651871740939725, 30.44471234641811819 ) ) ;
#19892 = DIRECTION ( 'NONE',  ( 1.000000000000000000, 0.000000000000000000, 0.000000000000000000 ) ) ;
#19893 = CARTESIAN_POINT ( 'NONE',  ( 43.01140435219951286, 102.5344580088725763, 39.21067981925356349 ) ) ;
#19894 = CARTESIAN_POINT ( 'NONE',  ( -153.0531000319306827, -177.1622583705452314, 39.65701158161630957 ) ) ;
#19895 = CARTESIAN_POINT ( 'NONE',  ( -161.4692556286852607, -182.6391397928654214, 46.40781461928724383 ) ) ;
#19896 =( BOUNDED_CURVE ( )  B_SPLINE_CURVE ( 2, ( #4971, #8717, #18844, #16857, #6747, #10370, #5081, #18526, #18420, #1771, #11683, #3318, #11795 ),
 .UNSPECIFIED., .F., .T. ) 
 B_SPLINE_CURVE_WITH_KNOTS ( ( 3, 2, 2, 2, 2, 2, 3 ),
 ( 0.2279411764705882304, 0.2294117647058823428, 0.2323529411764705954, 0.2352941176470588203, 0.2382352941176470451, 0.2411764705882352977, 0.2426470588235294101 ),
 .UNSPECIFIED. ) 
 CURVE ( )  GEOMETRIC_REPRESENTATION_ITEM ( )  RATIONAL_B_SPLINE_CURVE ( ( 0.9755282581475768211, 0.9755282581475768211, 1.000000000000000000, 0.9510565162951535312, 1.000000000000000000, 0.9510565162951535312, 1.000000000000000000, 0.9510565162951535312, 1.000000000000000000, 0.9510565162951535312, 1.000000000000000000, 0.9755282581475768211, 0.9755282581475768211 ) ) 
 REPRESENTATION_ITEM ( '' )  );
#19897 = ADVANCED_FACE ( 'NONE', ( #10297 ), #18878, .T. ) ;
#19898 = CARTESIAN_POINT ( 'NONE',  ( 38.01140435219952707, 156.8604996726487855, 35.83527830041809636 ) ) ;
#19899 = CARTESIAN_POINT ( 'NONE',  ( 47.05648932407426344, 93.98445800887257917, 37.14960608071593384 ) ) ;
#19900 = CARTESIAN_POINT ( 'NONE',  ( -154.3824083646099439, -190.2938272943107449, 58.62277379824867296 ) ) ;
#19901 = CARTESIAN_POINT ( 'NONE',  ( 47.05648932407426344, 121.5844580088725735, 31.27175355779120025 ) ) ;
#19902 = CARTESIAN_POINT ( 'NONE',  ( 41.64333658814960870, 104.7797705074273154, 30.00020018409699318 ) ) ;
#19903 = CARTESIAN_POINT ( 'NONE',  ( 48.57925227495098852, 92.17995633088730756, 20.19957357060707182 ) ) ;
#19904 = CARTESIAN_POINT ( 'NONE',  ( -142.0420953463935803, -183.2438272943107336, 46.59394152635518793 ) ) ;
#19905 = CARTESIAN_POINT ( 'NONE',  ( 41.64333658814960870, 89.51518717409399528, 30.00020018409699318 ) ) ;
#19906 = CARTESIAN_POINT ( 'NONE',  ( 43.01140435219951286, 85.46049967264872294, 39.21067981925356349 ) ) ;
#19907 = CIRCLE ( 'NONE', #6901, 10.00000000000000888 ) ;
#19908 = EDGE_LOOP ( 'NONE', ( #1383, #14063, #2572, #10317 ) ) ;
#19909 = CARTESIAN_POINT ( 'NONE',  ( 48.01140435219951996, 128.0604996726487457, 35.83527830041809636 ) ) ;
#19910 = DIRECTION ( 'NONE',  ( -1.000000000000000000, 0.000000000000000000, 0.000000000000000000 ) ) ;
#19911 = CARTESIAN_POINT ( 'NONE',  ( 40.27526882409969744, 143.9297705074273210, 30.44471234641812174 ) ) ;
#19912 = CARTESIAN_POINT ( 'NONE',  ( 14.99696000743431235, 117.4761687382565327, -3.934212988072375516 ) ) ;
#19913 = CARTESIAN_POINT ( 'NONE',  ( 40.27526882409969744, 66.82977050742731251, 37.97664729208901235 ) ) ;
#19914 = ORIENTED_EDGE ( 'NONE', *, *, #4612, .F. ) ;
#19915 = CARTESIAN_POINT ( 'NONE',  ( 40.27526882409969033, 146.9297705074273210, 30.44471234641811819 ) ) ;
#19916 = CARTESIAN_POINT ( 'NONE',  ( 48.01140435219951996, 152.3604996726487570, 32.58608133808903773 ) ) ;
#19917 = AXIS2_PLACEMENT_3D ( 'NONE', #9734, #8077, #19985 ) ;
#19918 = CARTESIAN_POINT ( 'NONE',  ( 44.55648932407425633, 106.6104996726487428, 38.96596240072933170 ) ) ;
#19919 = CARTESIAN_POINT ( 'NONE',  ( 40.27526882409969033, 65.66518717409398675, 30.44471234641811819 ) ) ;
#19920 = DIRECTION ( 'NONE',  ( 0.000000000000000000, 1.000000000000000000, 0.000000000000000000 ) ) ;
#19921 = CARTESIAN_POINT ( 'NONE',  ( -159.0959885057557983, -161.1938272943107222, 44.11586579668791330 ) ) ;
#19922 = CARTESIAN_POINT ( 'NONE',  ( 163.4517194221884040, 198.8869265230379995, -5.999999999999976019 ) ) ;
#19923 = CARTESIAN_POINT ( 'NONE',  ( -145.2889157411863721, -176.6130981290892805, 41.15050349809590102 ) ) ;
#19924 =( NAMED_UNIT ( * ) PLANE_ANGLE_UNIT ( ) SI_UNIT ( $, .RADIAN. ) );
#19925 = CARTESIAN_POINT ( 'NONE',  ( -151.4692556286852607, -192.2391397928655010, 39.65701158161629536 ) ) ;
#19926 = CARTESIAN_POINT ( 'NONE',  ( 41.46631938032478359, 156.3844580088725706, 38.96596240072933170 ) ) ;
#19927 = CARTESIAN_POINT ( 'NONE',  ( 47.43856463449117200, 134.0297705074273154, 32.77220824515698183 ) ) ;
#19928 = CARTESIAN_POINT ( 'NONE',  ( 24.18607167610233333, 148.5957190367184353, 16.19189608183989648 ) ) ;
#19929 = CARTESIAN_POINT ( 'NONE',  ( 44.37947211624943833, 115.0151871740940095, 38.42115945441014446 ) ) ;
#19930 = EDGE_CURVE ( 'NONE', #7143, #20168, #8620, .T. ) ;
#19931 = DIRECTION ( 'NONE',  ( 0.000000000000000000, 0.000000000000000000, 1.000000000000000000 ) ) ;
#19932 = LINE ( 'NONE', #8250, #21198 ) ;
#19933 = VECTOR ( 'NONE', #18150, 1000.000000000000000 ) ;
#19934 = CARTESIAN_POINT ( 'NONE',  ( 43.01140435219951996, 170.7104996726487514, 29.21067981925357060 ) ) ;
#19935 = AXIS2_PLACEMENT_3D ( 'NONE', #487, #7225, #386 ) ;
#19936 = CARTESIAN_POINT ( 'NONE',  ( 63.19260820189420969, 92.35335041358771946, 0.6293402173502762320 ) ) ;
#19937 = CARTESIAN_POINT ( 'NONE',  ( 34.17400395940548918, 146.6865494356538875, -10.43883331896520694 ) ) ;
#19938 = DIRECTION ( 'NONE',  ( 0.000000000000000000, 0.000000000000000000, 1.000000000000000000 ) ) ;
#19939 = CARTESIAN_POINT ( 'NONE',  ( 47.43856463449117911, 97.72977050742730398, 35.64915139335015937 ) ) ;
#19940 = VECTOR ( 'NONE', #6295, 1000.000000000000000 ) ;
#19941 = VERTEX_POINT ( 'NONE', #18774 ) ;
#19942 = FACE_OUTER_BOUND ( 'NONE', #19563, .T. ) ;
#19943 = VERTEX_POINT ( 'NONE', #17210 ) ;
#19944 = CARTESIAN_POINT ( 'NONE',  ( 48.01140435219951996, 82.43445800887258201, 32.58608133808903773 ) ) ;
#19945 = DIRECTION ( 'NONE',  ( 0.000000000000000000, 0.000000000000000000, 1.000000000000000000 ) ) ;
#19946 = ADVANCED_FACE ( 'NONE', ( #257, #16999 ), #8861, .F. ) ;
#19947 = CARTESIAN_POINT ( 'NONE',  ( 46.10157429594899270, 142.7604996726487343, 38.46393386101376421 ) ) ;
#19949 = CARTESIAN_POINT ( 'NONE',  ( 50.95956618318000864, 146.8798181090472212, 5.232242258870305918 ) ) ;
#19948 = CARTESIAN_POINT ( 'NONE',  ( 40.27526882409969033, 92.66518717409398675, 30.44471234641811819 ) ) ;
#19950 = AXIS2_PLACEMENT_3D ( 'NONE', #19614, #9378, #14214 ) ;
#19951 = CARTESIAN_POINT ( 'NONE',  ( -142.0420953463935803, -165.8084106276440366, 52.72008163687743831 ) ) ;
#19952 = CARTESIAN_POINT ( 'NONE',  ( -151.4692556286852891, -194.6438272943107393, 39.74470866294723947 ) ) ;
#19954 = DIRECTION ( 'NONE',  ( -0.000000000000000000, -1.000000000000000000, -0.000000000000000000 ) ) ;
#19953 = CARTESIAN_POINT ( 'NONE',  ( 43.01140435219951286, 62.03445800887256922, 29.21067981925356705 ) ) ;
#19955 = DIRECTION ( 'NONE',  ( -0.3450121214752278065, 0.9385982292947087080, -0.000000000000000000 ) ) ;
#19956 = AXIS2_PLACEMENT_3D ( 'NONE', #14414, #17393, #15633 ) ;
#19957 = CARTESIAN_POINT ( 'NONE',  ( 38.01140435219952707, 147.5604996726487173, 32.58608133808903773 ) ) ;
#19958 = CARTESIAN_POINT ( 'NONE',  ( 43.01140435219951286, 79.46049967264875136, 39.21067981925356349 ) ) ;
#19959 = AXIS2_PLACEMENT_3D ( 'NONE', #18223, #14692, #9422 ) ;
#19960 = CARTESIAN_POINT ( 'NONE',  ( 38.58424406990784661, 60.26518717409400239, 35.64915139335016647 ) ) ;
#19961 = CARTESIAN_POINT ( 'NONE',  ( 39.92123440845005433, 63.23445800887257917, 38.46393386101375711 ) ) ;
#19962 = CARTESIAN_POINT ( 'NONE',  ( 76.81974253126139729, 125.2811442093199616, -1.589308178208348910 ) ) ;
#19963 = CARTESIAN_POINT ( 'NONE',  ( 40.27526882409969744, 143.6651871740940294, 30.44471234641812174 ) ) ;
#19964 = CARTESIAN_POINT ( 'NONE',  ( -143.8425227516148084, -165.0938272943107279, 44.11586579668791330 ) ) ;
#19965 = CARTESIAN_POINT ( 'NONE',  ( -151.4692556286852891, -170.9084106276440593, 39.74470866294723947 ) ) ;
#19966 = VERTEX_POINT ( 'NONE', #17722 ) ;
#19967 = CARTESIAN_POINT ( 'NONE',  ( 38.96631938032478359, 77.48445800887257917, 31.27175355779120025 ) ) ;
#19968 =( BOUNDED_CURVE ( )  B_SPLINE_CURVE ( 2, ( #16734, #14859, #15200, #8049, #3300, #19952, #4955, #14967, #11663, #14753, #3076, #10028, #20175, #5065, #13541, #18401, #103, #6381, #4723, #10140, #18287, #11778, #3190, #13404, #21494, #13111, #1645, #6835, #18507, #3418, #20276, #6731, #11443, #8377, #18169, #16843, #11889, #19833, #2963, #9813, #16509, #1756, #13437, #8491, #15086, #5169, #1426, #9703, #16403, #8154, #1314, #21606, #6496, #16625, #13215, #4838, #11559, #9919, #1534, #8267, #21714, #6616, #13332, #20068, #17166, #10466, #8918, #18830, #1862, #6942, #425, #7266, #12098, #3736, #12208, #18943, #17057, #20814, #3950, #3843, #20706, #8703, #528, #13967, #5589, #10570, #12314, #20598, #5704, #10676, #1969, #20382, #2183, #13648, #10354, #10248, #15423, #8592, #15621, #5279, #7375, #5483, #19050, #16947, #3522, #17380, #20493, #2080, #641, #5382, #2285, #18723, #8811, #18618, #7157, #9024, #15522, #13860, #17271, #15736, #318, #14076, #15311, #203, #11993, #7047, #3631, #13753, #7804, #6023, #21251, #14402, #14616, #4474, #17597, #14184, #17810, #747, #4165, #4055, #2503, #9346, #6131, #2827, #4366, #21139, #14510, #10783, #19154, #12860, #14290, #19368, #16273, #21035, #9462, #12536, #4265, #21354, #15944, #5918, #2720, #20923, #9567, #12428, #2608, #19581, #12646, #17490, #19265, #11097, #9245, #1178, #2400, #12754, #7591, #19474, #16050, #16162, #9136, #10894, #1074, #11203, #10993, #15836, #7913, #17703, #17918, #7482, #7703, #854, #5805, #960, #3272, #11306, #16376, #4929, #10111, #21797, #1617, #18481, #10004, #13413, #16708, #21689, #19809, #18033, #6243, #16818, #1731, #4698, #8349, #15060, #6706, #18370, #8465, #9677, #20147, #15173, #2939, #5040, #11641, #12972, #14730, #11749, #13189, #6587, #1289, #3385, #19921, #19698, #4586, #8023, #21465, #4810, #11532, #6356, #6467, #13080, #11416, #20043, #18141, #3050, #9787, #16483, #1399, #8128, #14831, #21576, #18260, #3163, #9893, #16593, #1511, #8240, #14942, #13305, #3817, #20573, #179, #13729, #12288, #7241, #3499, #504, #15598, #20466, #5359, #6914, #10441 ),
 .UNSPECIFIED., .F., .F. ) 
 B_SPLINE_CURVE_WITH_KNOTS ( ( 3, 2, 2, 2, 2, 2, 2, 2, 2, 2, 2, 2, 2, 2, 2, 2, 2, 2, 2, 2, 2, 2, 2, 2, 2, 2, 2, 2, 2, 2, 2, 2, 2, 2, 2, 2, 2, 2, 2, 2, 2, 2, 2, 2, 2, 2, 2, 2, 2, 2, 2, 2, 2, 2, 2, 2, 2, 2, 2, 2, 2, 2, 2, 2, 2, 2, 2, 2, 2, 2, 2, 2, 2, 2, 2, 2, 2, 2, 2, 2, 2, 2, 2, 2, 2, 2, 2, 2, 2, 2, 2, 2, 2, 2, 2, 2, 2, 2, 2, 2, 2, 2, 2, 2, 2, 2, 2, 2, 2, 2, 2, 2, 2, 2, 2, 2, 2, 2, 2, 2, 2, 2, 2, 2, 2, 2, 2, 2, 2, 2, 2, 2, 2, 2, 3 ),
 ( 0.000000000000000000, 0.007142857142857142634, 0.01428571428571428527, 0.02142857142857142877, 0.02857142857142857054, 0.03571428571428571230, 0.04285714285714285754, 0.05000000000000000278, 0.05714285714285714107, 0.06428571428571427937, 0.07142857142857142461, 0.07857142857142856984, 0.08571428571428571508, 0.09285714285714286031, 0.1000000000000000056, 0.1071428571428571369, 0.1142857142857142821, 0.1214285714285714274, 0.1285714285714285587, 0.1357142857142857040, 0.1428571428571428492, 0.1499999999999999944, 0.1571428571428571397, 0.1642857142857142849, 0.1714285714285714302, 0.1785714285714285754, 0.1857142857142857206, 0.1928571428571428659, 0.2000000000000000111, 0.2071428571428571841, 0.2142857142857142738, 0.2214285714285714191, 0.2285714285714285643, 0.2357142857142857373, 0.2428571428571428548, 0.2500000000000000000, 0.2571428571428571175, 0.2642857142857142905, 0.2714285714285714080, 0.2785714285714285254, 0.2857142857142856984, 0.2928571428571428714, 0.2999999999999999889, 0.3071428571428571619, 0.3142857142857142794, 0.3214285714285714524, 0.3285714285714285698, 0.3357142857142856318, 0.3428571428571428603, 0.3499999999999999778, 0.3571428571428571508, 0.3642857142857142683, 0.3714285714285714413, 0.3785714285714285587, 0.3857142857142857317, 0.3928571428571428492, 0.4000000000000000222, 0.4071428571428571397, 0.4142857142857143682, 0.4214285714285714302, 0.4285714285714285476, 0.4357142857142857206, 0.4428571428571428381, 0.4500000000000000111, 0.4571428571428571286, 0.4642857142857143016, 0.4714285714285714746, 0.4785714285714285920, 0.4857142857142857095, 0.4928571428571428825, 0.5000000000000000000, 0.5071428571428571175, 0.5142857142857142350, 0.5214285714285714635, 0.5285714285714285809, 0.5357142857142856984, 0.5428571428571428159, 0.5500000000000000444, 0.5571428571428570509, 0.5642857142857142794, 0.5714285714285713969, 0.5785714285714286254, 0.5857142857142857428, 0.5928571428571428603, 0.5999999999999999778, 0.6071428571428570953, 0.6142857142857143238, 0.6214285714285714413, 0.6285714285714285587, 0.6357142857142856762, 0.6428571428571429047, 0.6500000000000000222, 0.6571428571428571397, 0.6642857142857142572, 0.6714285714285712636, 0.6785714285714286031, 0.6857142857142857206, 0.6928571428571428381, 0.6999999999999999556, 0.7071428571428571841, 0.7142857142857143016, 0.7214285714285714191, 0.7285714285714285365, 0.7357142857142857650, 0.7428571428571428825, 0.7500000000000001110, 0.7571428571428571175, 0.7642857142857142350, 0.7714285714285714635, 0.7785714285714285809, 0.7857142857142856984, 0.7928571428571428159, 0.8000000000000000444, 0.8071428571428571619, 0.8142857142857142794, 0.8214285714285713969, 0.8285714285714287364, 0.8357142857142857428, 0.8428571428571428603, 0.8499999999999999778, 0.8571428571428570953, 0.8642857142857143238, 0.8714285714285714413, 0.8785714285714285587, 0.8857142857142856762, 0.8928571428571429047, 0.9000000000000000222, 0.9071428571428571397, 0.9142857142857142572, 0.9214285714285713746, 0.9285714285714286031, 0.9357142857142857206, 0.9428571428571429491, 0.9499999999999999556, 0.9523897199067098418 ),
 .UNSPECIFIED. ) 
 CURVE ( )  GEOMETRIC_REPRESENTATION_ITEM ( )  RATIONAL_B_SPLINE_CURVE ( ( 1.000000000000000000, 0.9510565162951535312, 1.000000000000000000, 0.9510565162951535312, 1.000000000000000000, 0.9510565162951535312, 1.000000000000000000, 0.9510565162951535312, 1.000000000000000000, 0.9510565162951535312, 1.000000000000000000, 0.9510565162951535312, 1.000000000000000000, 0.9510565162951535312, 1.000000000000000000, 0.9510565162951535312, 1.000000000000000000, 0.9510565162951535312, 1.000000000000000000, 0.9510565162951535312, 1.000000000000000000, 0.9510565162951535312, 1.000000000000000000, 0.9510565162951535312, 1.000000000000000000, 0.9510565162951535312, 1.000000000000000000, 0.9510565162951535312, 1.000000000000000000, 0.9510565162951535312, 1.000000000000000000, 0.9510565162951535312, 1.000000000000000000, 0.9510565162951535312, 1.000000000000000000, 0.9510565162951535312, 1.000000000000000000, 0.9510565162951535312, 1.000000000000000000, 0.9510565162951535312, 1.000000000000000000, 0.9510565162951535312, 1.000000000000000000, 0.9510565162951535312, 1.000000000000000000, 0.9510565162951535312, 1.000000000000000000, 0.9510565162951535312, 1.000000000000000000, 0.9510565162951535312, 1.000000000000000000, 0.9510565162951535312, 1.000000000000000000, 0.9510565162951535312, 1.000000000000000000, 0.9510565162951535312, 1.000000000000000000, 0.9510565162951535312, 1.000000000000000000, 0.9510565162951535312, 1.000000000000000000, 0.9510565162951535312, 1.000000000000000000, 0.9510565162951535312, 1.000000000000000000, 0.9510565162951535312, 1.000000000000000000, 0.9510565162951535312, 1.000000000000000000, 0.9510565162951535312, 1.000000000000000000, 0.9510565162951535312, 1.000000000000000000, 0.9510565162951535312, 1.000000000000000000, 0.9510565162951535312, 1.000000000000000000, 0.9510565162951535312, 1.000000000000000000, 0.9510565162951535312, 1.000000000000000000, 0.9510565162951535312, 1.000000000000000000, 0.9510565162951535312, 1.000000000000000000, 0.9510565162951535312, 1.000000000000000000, 0.9510565162951535312, 1.000000000000000000, 0.9510565162951535312, 1.000000000000000000, 0.9510565162951535312, 1.000000000000000000, 0.9510565162951535312, 1.000000000000000000, 0.9510565162951535312, 1.000000000000000000, 0.9510565162951535312, 1.000000000000000000, 0.9510565162951535312, 1.000000000000000000, 0.9510565162951535312, 1.000000000000000000, 0.9510565162951535312, 1.000000000000000000, 0.9510565162951535312, 1.000000000000000000, 0.9510565162951535312, 1.000000000000000000, 0.9510565162951535312, 1.000000000000000000, 0.9510565162951535312, 1.000000000000000000, 0.9510565162951535312, 1.000000000000000000, 0.9510565162951535312, 1.000000000000000000, 0.9510565162951535312, 1.000000000000000000, 0.9510565162951535312, 1.000000000000000000, 0.9510565162951535312, 1.000000000000000000, 0.9510565162951535312, 1.000000000000000000, 0.9510565162951535312, 1.000000000000000000, 0.9510565162951535312, 1.000000000000000000, 0.9510565162951535312, 1.000000000000000000, 0.9510565162951535312, 1.000000000000000000, 0.9510565162951535312, 1.000000000000000000, 0.9510565162951535312, 1.000000000000000000, 0.9510565162951535312, 1.000000000000000000, 0.9510565162951535312, 1.000000000000000000, 0.9510565162951535312, 1.000000000000000000, 0.9510565162951535312, 1.000000000000000000, 0.9510565162951535312, 1.000000000000000000, 0.9510565162951535312, 1.000000000000000000, 0.9510565162951535312, 1.000000000000000000, 0.9510565162951535312, 1.000000000000000000, 0.9510565162951535312, 1.000000000000000000, 0.9510565162951535312, 1.000000000000000000, 0.9510565162951535312, 1.000000000000000000, 0.9510565162951535312, 1.000000000000000000, 0.9510565162951535312, 1.000000000000000000, 0.9510565162951535312, 1.000000000000000000, 0.9510565162951535312, 1.000000000000000000, 0.9510565162951535312, 1.000000000000000000, 0.9510565162951535312, 1.000000000000000000, 0.9510565162951535312, 1.000000000000000000, 0.9510565162951535312, 1.000000000000000000, 0.9510565162951535312, 1.000000000000000000, 0.9510565162951535312, 1.000000000000000000, 0.9510565162951535312, 1.000000000000000000, 0.9510565162951535312, 1.000000000000000000, 0.9510565162951535312, 1.000000000000000000, 0.9510565162951535312, 1.000000000000000000, 0.9510565162951535312, 1.000000000000000000, 0.9510565162951535312, 1.000000000000000000, 0.9510565162951535312, 1.000000000000000000, 0.9510565162951535312, 1.000000000000000000, 0.9510565162951535312, 1.000000000000000000, 0.9510565162951535312, 1.000000000000000000, 0.9510565162951535312, 1.000000000000000000, 0.9510565162951535312, 1.000000000000000000, 0.9510565162951535312, 1.000000000000000000, 0.9510565162951535312, 1.000000000000000000, 0.9510565162951535312, 1.000000000000000000, 0.9510565162951535312, 1.000000000000000000, 0.9510565162951535312, 1.000000000000000000, 0.9510565162951535312, 1.000000000000000000, 0.9510565162951535312, 1.000000000000000000, 0.9510565162951535312, 1.000000000000000000, 0.9510565162951535312, 1.000000000000000000, 0.9510565162951535312, 1.000000000000000000, 0.9510565162951535312, 1.000000000000000000, 0.9510565162951535312, 1.000000000000000000, 0.9510565162951535312, 1.000000000000000000, 0.9510565162951535312, 1.000000000000000000, 0.9510565162951535312, 1.000000000000000000, 0.9510565162951535312, 1.000000000000000000, 0.9510565162951535312, 1.000000000000000000, 0.9510565162951535312, 1.000000000000000000, 0.9510565162951535312, 1.000000000000000000, 0.9510565162951535312, 1.000000000000000000, 0.9510565162951535312, 1.000000000000000000, 0.9510565162951535312, 1.000000000000000000, 0.9510565162951535312, 1.000000000000000000, 0.9510565162951535312, 1.000000000000000000, 0.9510565162951535312, 1.000000000000000000, 0.9510565162951535312, 1.000000000000000000, 0.9510565162951535312, 1.000000000000000000, 0.9510565162951535312, 1.000000000000000000, 0.9510565162951535312, 1.000000000000000000, 0.9510565162951535312, 1.000000000000000000, 0.9510565162951535312, 1.000000000000000000, 0.9510565162951535312, 1.000000000000000000, 0.9836254295761526212, 0.9782074374858980015 ) ) 
 REPRESENTATION_ITEM ( '' )  );
#19969 = CARTESIAN_POINT ( 'NONE',  ( -160.8964159109769696, -161.3084106276440082, 46.59394152635518793 ) ) ;
#19970 = CARTESIAN_POINT ( 'NONE',  ( 22.58852954093744714, 92.33198060352846426, 14.04912700239559520 ) ) ;
#19971 = FACE_OUTER_BOUND ( 'NONE', #20568, .T. ) ;
#19972 = CARTESIAN_POINT ( 'NONE',  ( 38.58424406990784661, 122.9651871740939981, 32.77220824515698183 ) ) ;
#19973 = CARTESIAN_POINT ( 'NONE',  ( 44.19315180539718568, 85.77372119115894122, -12.70412401877768005 ) ) ;
#19974 = AXIS2_PLACEMENT_3D ( 'NONE', #14585, #12944, #1482 ) ;
#19975 = VERTEX_POINT ( 'NONE', #7611 ) ;
#19976 = VERTEX_POINT ( 'NONE', #12259 ) ;
#19977 = CARTESIAN_POINT ( 'NONE',  ( 38.01140435219952707, 146.6344580088725991, 32.58608133808903773 ) ) ;
#19978 = ORIENTED_EDGE ( 'NONE', *, *, #21369, .T. ) ;
#19979 = CARTESIAN_POINT ( 'NONE',  ( 45.74753988029934249, 155.3297705074273267, 30.44471234641812174 ) ) ;
#19980 = CARTESIAN_POINT ( 'NONE',  ( 43.01140435219951286, 65.62977050742730967, 29.55568802177586463 ) ) ;
#19982 = CARTESIAN_POINT ( 'NONE',  ( 19.85370653151704090, 103.8158566922722486, 8.489678972899794118 ) ) ;
#19981 = CARTESIAN_POINT ( 'NONE',  ( 45.74753988029933538, 121.1651871740939725, 37.97664729208901946 ) ) ;
#19983 = CIRCLE ( 'NONE', #3785, 9.000000000000007105 ) ;
#19984 = CARTESIAN_POINT ( 'NONE',  ( 38.01140435219951996, 81.56049967264873146, 32.58608133808903773 ) ) ;
#19985 = DIRECTION ( 'NONE',  ( 1.000000000000000000, 0.000000000000000000, 0.000000000000000000 ) ) ;
#19986 = CARTESIAN_POINT ( 'NONE',  ( 38.96631938032478359, 145.0104996726487627, 37.14960608071593384 ) ) ;
#19987 = CARTESIAN_POINT ( 'NONE',  ( 38.01140435219952707, 138.7104996726487514, 34.21067981925357060 ) ) ;
#19988 = CARTESIAN_POINT ( 'NONE',  ( 38.58424406990784661, 84.26518717409399528, 35.64915139335016647 ) ) ;
#19989 = CARTESIAN_POINT ( 'NONE',  ( 38.01153310497667093, 144.4020013279858290, 34.53968432338326977 ) ) ;
#19990 = PRODUCT ( 'Handle Balance Tension Spring', 'Handle Balance Tension Spring', '', ( #20897 ) ) ;
#19991 = CARTESIAN_POINT ( 'NONE',  ( -159.5594255724347761, -185.7891397928654840, 43.77915905869157598 ) ) ;
#19992 = ORIENTED_EDGE ( 'NONE', *, *, #7368, .T. ) ;
#19993 = CARTESIAN_POINT ( 'NONE',  ( 44.37947211624943833, 67.27977050742731535, 38.42115945441014446 ) ) ;
#19994 = CARTESIAN_POINT ( 'NONE',  ( -142.0420953463935803, -195.5084106276440536, 46.59394152635518793 ) ) ;
#19995 = EDGE_CURVE ( 'NONE', #3266, #13122, #5327, .T. ) ;
#19996 = CARTESIAN_POINT ( 'NONE',  ( 9.656473946750173454, 127.6128973189080398, 2.339233609801092406 ) ) ;
#19997 = CARTESIAN_POINT ( 'NONE',  ( -142.0420953463935803, -189.8084106276440366, 52.72008163687743831 ) ) ;
#19998 = ORIENTED_EDGE ( 'NONE', *, *, #15163, .F. ) ;
#19999 = CARTESIAN_POINT ( 'NONE',  ( 45.74753988029933538, 152.0651871740939782, 30.44471234641811819 ) ) ;
#20000 = LINE ( 'NONE', #4665, #3940 ) ;
#20001 = CARTESIAN_POINT ( 'NONE',  ( 44.37947211624943833, 118.2797705074273296, 38.42115945441014446 ) ) ;
#20002 = CARTESIAN_POINT ( 'NONE',  ( 30.08091612619420729, 88.20954595054467973, -6.232194961517499188 ) ) ;
#20003 = VECTOR ( 'NONE', #21237, 1000.000000000000227 ) ;
#20004 = EDGE_LOOP ( 'NONE', ( #10613, #12470 ) ) ;
#20005 = CARTESIAN_POINT ( 'NONE',  ( 20.57499262110235350, 102.8243204193801432, -5.557751863727047770 ) ) ;
#20006 = EDGE_LOOP ( 'NONE', ( #10615, #686, #16040, #21080 ) ) ;
#20007 = CARTESIAN_POINT ( 'NONE',  ( 38.58424406990784661, 117.5297705074273011, 35.64915139335016647 ) ) ;
#20008 = AXIS2_PLACEMENT_3D ( 'NONE', #3425, #20282, #13338 ) ;
#20009 = PLANE ( 'NONE',  #9038 ) ;
#20010 = CARTESIAN_POINT ( 'NONE',  ( 43.01140435219951286, 86.62977050742730967, 29.55568802177586463 ) ) ;
#20011 = CARTESIAN_POINT ( 'NONE',  ( 43.01140435219951286, 152.3651871740940180, 29.55568802177586463 ) ) ;
#20012 = CARTESIAN_POINT ( 'NONE',  ( 43.10205244623161036, 154.1398065127551149, -10.16071067355346358 ) ) ;
#20013 = CARTESIAN_POINT ( 'NONE',  ( -130.4480969619997950, -126.9891397928655010, -72.64809332337412684 ) ) ;
#20014 = DIRECTION ( 'NONE',  ( -0.000000000000000000, -0.000000000000000000, -1.000000000000000000 ) ) ;
#20015 = CARTESIAN_POINT ( 'NONE',  ( -151.4692556286852891, -181.7391397928654726, 59.65701158161631668 ) ) ;
#20016 = CARTESIAN_POINT ( 'NONE',  ( -141.4692556286852891, -183.8391397928654669, 46.40781461928724383 ) ) ;
#20017 = CARTESIAN_POINT ( 'NONE',  ( 42.21948215057684450, 156.0373810949690210, 29.21067981925356705 ) ) ;
#20018 = LINE ( 'NONE', #21442, #15689 ) ;
#20019 = CARTESIAN_POINT ( 'NONE',  ( -154.3824083646099439, -193.2938272943107449, 58.62277379824867296 ) ) ;
#20020 = CONTEXT_DEPENDENT_SHAPE_REPRESENTATION ( #9430, #7656 ) ;
#20021 = CARTESIAN_POINT ( 'NONE',  ( 39.42975644700377558, 96.07977050742731251, 31.60846029578754468 ) ) ;
#20022 = CARTESIAN_POINT ( 'NONE',  ( 59.59119729515064279, 96.99641097138604096, 19.72329267725583080 ) ) ;
#20023 = CARTESIAN_POINT ( 'NONE',  ( -143.8425227516148084, -186.6938272943107222, 55.19815736654470584 ) ) ;
#20024 = ADVANCED_FACE ( 'NONE', ( #12045 ), #7206, .T. ) ;
#20025 = CARTESIAN_POINT ( 'NONE',  ( 39.42975644700377558, 84.41518717409400097, 36.81289934271958941 ) ) ;
#20026 = STYLED_ITEM ( 'NONE', ( #11229 ), #7141 ) ;
#20027 = DIRECTION ( 'NONE',  ( -1.000000000000000000, 0.000000000000000000, 0.000000000000000000 ) ) ;
#20028 = ORIENTED_EDGE ( 'NONE', *, *, #5555, .T. ) ;
#20029 = LINE ( 'NONE', #5241, #18220 ) ;
#20030 = CARTESIAN_POINT ( 'NONE',  ( 49.46632042442519861, 86.28835692931116341, 14.12497754236212977 ) ) ;
#20031 = CARTESIAN_POINT ( 'NONE',  ( 41.64333658814960870, 140.7797705074273154, 30.00020018409699318 ) ) ;
#20032 = CARTESIAN_POINT ( 'NONE',  ( 37.37095630934955892, 92.35886976769425871, -5.362784416626555029 ) ) ;
#20033 = CARTESIAN_POINT ( 'NONE',  ( 45.74753988029934249, 71.32977050742732672, 30.44471234641812174 ) ) ;
#20034 = ORIENTED_EDGE ( 'NONE', *, *, #18208, .F. ) ;
#20035 = CARTESIAN_POINT ( 'NONE',  ( 44.37947211624943833, 142.2797705074273154, 38.42115945441014446 ) ) ;
#20036 = CARTESIAN_POINT ( 'NONE',  ( 40.27526882409969033, 96.82977050742731251, 37.97664729208901946 ) ) ;
#20037 = CARTESIAN_POINT ( 'NONE',  ( 44.55648932407425633, 152.8104996726487457, 29.45539723777780239 ) ) ;
#20038 = EDGE_CURVE ( 'NONE', #16317, #17856, #2091, .T. ) ;
#20039 = ADVANCED_FACE ( 'NONE', ( #2233, #20542 ), #18993, .T. ) ;
#20040 = CARTESIAN_POINT ( 'NONE',  ( 38.96631938032478359, 114.4104996726487400, 31.27175355779120025 ) ) ;
#20041 = CARTESIAN_POINT ( 'NONE',  ( 40.27526882409969033, 69.56518717409400665, 37.97664729208901946 ) ) ;
#20042 = CARTESIAN_POINT ( 'NONE',  ( 42.21948215057684450, 95.11133943119284595, 29.21067981925356705 ) ) ;
#20043 = CARTESIAN_POINT ( 'NONE',  ( -142.0420953463935803, -159.5438272943107449, 52.72008163687743831 ) ) ;
#20044 = DIRECTION ( 'NONE',  ( 1.000000000000000000, 0.000000000000000000, 0.000000000000000000 ) ) ;
#20045 = CARTESIAN_POINT ( 'NONE',  ( -157.6495955161842062, -178.1130981290893374, 58.16351966513671812 ) ) ;
#20046 = CARTESIAN_POINT ( 'NONE',  ( 43.01140435219951996, 10.71049967264875491, 34.21067981925357060 ) ) ;
#20047 = CARTESIAN_POINT ( 'NONE',  ( 48.01140435219951996, 154.1344580088725991, 35.83527830041810347 ) ) ;
#20048 = CARTESIAN_POINT ( 'NONE',  ( 38.58424406990784661, 126.5297705074272727, 35.64915139335016647 ) ) ;
#20049 = CARTESIAN_POINT ( 'NONE',  ( 77.30322022806339533, 121.1324128411339984, 11.54915785461027511 ) ) ;
#20050 = CARTESIAN_POINT ( 'NONE',  ( 41.64333658814960870, 117.7151871740939981, 38.42115945441014446 ) ) ;
#20051 = CARTESIAN_POINT ( 'NONE',  ( 126.8576204525573274, -126.9891397928655010, 67.64809332337412684 ) ) ;
#20052 = CARTESIAN_POINT ( 'NONE',  ( 47.05648932407426344, 140.5104996726487627, 31.27175355779120025 ) ) ;
#20053 = CARTESIAN_POINT ( 'NONE',  ( 22.33864107606189719, 92.72021074822440312, 2.057911645927444244 ) ) ;
#20054 = CARTESIAN_POINT ( 'NONE',  ( 24.77189431714078083, 141.4131305960171687, 3.132649400142189844 ) ) ;
#20055 = CARTESIAN_POINT ( 'NONE',  ( 43.01140435219951996, 2.710499672648754466, 59.21067981925356349 ) ) ;
#20056 = VECTOR ( 'NONE', #20647, 999.9999999999998863 ) ;
#20057 = CARTESIAN_POINT ( 'NONE',  ( 45.74753988029934249, 94.42977050742733525, 37.97664729208901235 ) ) ;
#20058 = EDGE_LOOP ( 'NONE', ( #14934, #5957, #11656, #12600 ) ) ;
#20059 = CARTESIAN_POINT ( 'NONE',  ( 47.05648932407426344, 145.5844580088725877, 31.27175355779120025 ) ) ;
#20060 = ORIENTED_EDGE ( 'NONE', *, *, #5076, .F. ) ;
#20061 = CARTESIAN_POINT ( 'NONE',  ( 38.01140435219951996, 80.93445800887256780, 35.83527830041810347 ) ) ;
#20062 = CYLINDRICAL_SURFACE ( 'NONE', #8783, 10.00000000000000888 ) ;
#20063 = ADVANCED_FACE ( 'NONE', ( #1908 ), #17324, .T. ) ;
#20064 = CARTESIAN_POINT ( 'NONE',  ( 44.55648932407425633, 142.6104996726487570, 38.96596240072933170 ) ) ;
#20066 = CARTESIAN_POINT ( 'NONE',  ( 69.68093098098093208, 128.8215514297462789, 6.303499042945750475 ) ) ;
#20065 = CARTESIAN_POINT ( 'NONE',  ( 45.74753988029933538, 98.06518717409397823, 30.44471234641811819 ) ) ;
#20067 = CARTESIAN_POINT ( 'NONE',  ( -143.8425227516148084, -168.9584106276440423, 55.19815736654470584 ) ) ;
#20068 = CARTESIAN_POINT ( 'NONE',  ( -145.6429501568359797, -185.9438272943107506, 41.63779006702063867 ) ) ;
#20070 = DIRECTION ( 'NONE',  ( -1.000000000000000000, 0.000000000000000000, 0.000000000000000000 ) ) ;
#20069 = CARTESIAN_POINT ( 'NONE',  ( -159.5594255724347761, -166.8630981290893089, 43.77915905869157598 ) ) ;
#20071 = CARTESIAN_POINT ( 'NONE',  ( 42.21948215057684450, 106.3836182503284533, 39.21067981925355639 ) ) ;
#20072 = COLOUR_RGB ( '', 0.08235294, 0.09019608, 0.10196078) ;
#20073 = LINE ( 'NONE', #4959, #18086 ) ;
#20074 = CARTESIAN_POINT ( 'NONE',  ( 38.96631938032478359, 79.01049967264873430, 37.14960608071593384 ) ) ;
#20075 = CARTESIAN_POINT ( 'NONE',  ( 47.43856463449117200, 64.46518717409398391, 35.64915139335016647 ) ) ;
#20076 = CARTESIAN_POINT ( 'NONE',  ( 11.67247064774405452, 106.1322524520788875, 1.624861436118421043 ) ) ;
#20077 = CARTESIAN_POINT ( 'NONE',  ( 41.64333658814960870, 144.7151871740940123, 38.42115945441014446 ) ) ;
#20078 = CARTESIAN_POINT ( 'NONE',  ( -142.0420953463936087, -159.3938272943107393, 49.65701158161630957 ) ) ;
#20079 = CARTESIAN_POINT ( 'NONE',  ( -145.6429501568359797, -177.2084106276440707, 41.63779006702063867 ) ) ;
#20080 = ORIENTED_EDGE ( 'NONE', *, *, #4507, .T. ) ;
#20081 = CARTESIAN_POINT ( 'NONE',  ( 38.01140435219952707, 77.78445800887259054, 34.21067981925357060 ) ) ;
#20082 = CARTESIAN_POINT ( 'NONE',  ( -145.6429501568359797, -159.2084106276439854, 41.63779006702063867 ) ) ;
#20083 = CARTESIAN_POINT ( 'NONE',  ( 65.22477088018504787, 102.4029861919955948, -1.586113490162427864 ) ) ;
#20084 = CARTESIAN_POINT ( 'NONE',  ( 93.25569916848381524, 126.0916958004080755, -19.99999999999997868 ) ) ;
#20085 = CARTESIAN_POINT ( 'NONE',  ( 40.27526882409969033, 122.6651871740939725, 30.44471234641811819 ) ) ;
#20086 = CARTESIAN_POINT ( 'NONE',  ( 33.21234449867455396, 152.6251194638087725, -9.489586336475131390 ) ) ;
#20087 = VERTEX_POINT ( 'NONE', #12667 ) ;
#20088 = ORIENTED_EDGE ( 'NONE', *, *, #14863, .F. ) ;
#20089 = CARTESIAN_POINT ( 'NONE',  ( -151.4692556286852607, -161.3130981290892976, 39.65701158161629536 ) ) ;
#20090 = EDGE_LOOP ( 'NONE', ( #14148, #16369, #7773, #18132 ) ) ;
#20091 = CARTESIAN_POINT ( 'NONE',  ( 47.43856463449118621, 157.8797705074273381, 34.21067981925357060 ) ) ;
#20092 = CARTESIAN_POINT ( 'NONE',  ( 40.27526882409969033, 66.82977050742732672, 37.97664729208901946 ) ) ;
#20094 = CARTESIAN_POINT ( 'NONE',  ( 26.10333545525518062, 97.33820528946348816, 8.132564544556878161 ) ) ;
#20093 = CARTESIAN_POINT ( 'NONE',  ( 43.01140435219951286, 129.8651871740940180, 38.86567161673127657 ) ) ;
#20095 = CARTESIAN_POINT ( 'NONE',  ( 38.01140435219951996, 78.56049967264873146, 32.58608133808903773 ) ) ;
#20096 = CARTESIAN_POINT ( 'NONE',  ( -176.9699209214867608, -136.9891397928655010, 30.00000000000000000 ) ) ;
#20097 = CARTESIAN_POINT ( 'NONE',  ( 43.01140435219951996, 10.71049967264875491, 34.21067981925357060 ) ) ;
#20098 = CARTESIAN_POINT ( 'NONE',  ( 43.01140435219951286, 118.4604996726487371, 39.21067981925356349 ) ) ;
#20099 =( BOUNDED_CURVE ( )  B_SPLINE_CURVE ( 2, ( #15917, #5677, #4031, #19341, #16138, #9219, #830, #16022, #934, #14161, #17892, #1047, #7781 ),
 .UNSPECIFIED., .F., .F. ) 
 B_SPLINE_CURVE_WITH_KNOTS ( ( 3, 2, 2, 2, 2, 2, 3 ),
 ( 0.8308823529411765163, 0.8323529411764706287, 0.8352941176470588536, 0.8382352941176470784, 0.8411764705882353033, 0.8441176470588235281, 0.8455882352941176405 ),
 .UNSPECIFIED. ) 
 CURVE ( )  GEOMETRIC_REPRESENTATION_ITEM ( )  RATIONAL_B_SPLINE_CURVE ( ( 0.9755282581475768211, 0.9755282581475768211, 1.000000000000000000, 0.9510565162951535312, 1.000000000000000000, 0.9510565162951535312, 1.000000000000000000, 0.9510565162951535312, 1.000000000000000000, 0.9510565162951535312, 1.000000000000000000, 0.9755282581475768211, 0.9755282581475768211 ) ) 
 REPRESENTATION_ITEM ( '' )  );
#20100 = CARTESIAN_POINT ( 'NONE',  ( 46.59305225739526435, 88.91518717409400097, 31.60846029578754468 ) ) ;
#20101 = CARTESIAN_POINT ( 'NONE',  ( 38.68091485423948939, 144.5292836280306972, 31.70594869545380945 ) ) ;
#20102 = DIRECTION ( 'NONE',  ( 0.9387810623359078566, 0.3426822732243069436, 0.03548206049944095664 ) ) ;
#20103 = ORIENTED_EDGE ( 'NONE', *, *, #21681, .F. ) ;
#20104 = CARTESIAN_POINT ( 'NONE',  ( 45.74753988029933538, 61.42977050742732104, 37.97664729208901946 ) ) ;
#20105 = CARTESIAN_POINT ( 'NONE',  ( -159.0959885057557983, -184.8584106276440480, 55.19815736654470584 ) ) ;
#20106 = CARTESIAN_POINT ( 'NONE',  ( 23.42018083028975184, 147.9700754799198705, 17.16443675223517573 ) ) ;
#20107 = CARTESIAN_POINT ( 'NONE',  ( -143.8425227516148084, -177.9584106276440707, 55.19815736654470584 ) ) ;
#20108 = VERTEX_POINT ( 'NONE', #10514 ) ;
#20109 = CARTESIAN_POINT ( 'NONE',  ( 43.01140435219951286, 158.3651871740939612, 29.55568802177586463 ) ) ;
#20110 = CARTESIAN_POINT ( 'NONE',  ( -149.8854112254399240, -159.3160212151857422, 39.65701158161629536 ) ) ;
#20111 = CARTESIAN_POINT ( 'NONE',  ( 41.64333658814960870, 111.9797705074273324, 38.42115945441014446 ) ) ;
#20112 = CARTESIAN_POINT ( 'NONE',  ( 48.01140435219951996, 154.2844580088725763, 34.21067981925357060 ) ) ;
#20113 = VERTEX_POINT ( 'NONE', #17106 ) ;
#20114 = CARTESIAN_POINT ( 'NONE',  ( 26.65597624659334031, 142.8797025615743337, -3.772066457372480475 ) ) ;
#20115 = ORIENTED_EDGE ( 'NONE', *, *, #3491, .T. ) ;
#20116 = CARTESIAN_POINT ( 'NONE',  ( 47.43856463449117200, 118.7297705074272898, 35.64915139335016647 ) ) ;
#20117 = CARTESIAN_POINT ( 'NONE',  ( 41.46631938032478359, 127.3104996726487315, 38.96596240072933170 ) ) ;
#20118 = CARTESIAN_POINT ( 'NONE',  ( 39.42975644700377558, 84.67977050742732104, 36.81289934271958941 ) ) ;
#20119 = CARTESIAN_POINT ( 'NONE',  ( 38.58424406990786082, 153.1151871740939896, 34.21067981925357060 ) ) ;
#20120 = CARTESIAN_POINT ( 'NONE',  ( 74.62708615766334219, 133.0342049366344384, -8.851289726714327344 ) ) ;
#20121 = DIRECTION ( 'NONE',  ( 0.9385982292947088190, 0.3450121214752278620, -0.000000000000000000 ) ) ;
#20122 = FACE_OUTER_BOUND ( 'NONE', #10887, .T. ) ;
#20123 = CARTESIAN_POINT ( 'NONE',  ( -141.4692556286852891, -178.1391397928654499, 52.90620854394536821 ) ) ;
#20124 = FACE_OUTER_BOUND ( 'NONE', #20006, .T. ) ;
#20125 = CARTESIAN_POINT ( 'NONE',  ( 131.0765927465021434, 198.5836349573982886, 14.00000000000001776 ) ) ;
#20126 = ITEM_DEFINED_TRANSFORMATION ( 'NONE', 'NONE', #18309,  #12657 ) ;
#20127 = CARTESIAN_POINT ( 'NONE',  ( 47.43856463449118621, 91.87977050742732388, 34.21067981925357060 ) ) ;
#20128 = CARTESIAN_POINT ( 'NONE',  ( 15.06790588970514833, 124.2609462974868677, 22.34264618625151044 ) ) ;
#20129 = CARTESIAN_POINT ( 'NONE',  ( -148.5561028927606344, -176.7938272943107165, 40.69124936498395328 ) ) ;
#20130 = CARTESIAN_POINT ( 'NONE',  ( 43.01140435219951286, 87.86518717409398960, 38.86567161673127657 ) ) ;
#20131 = LINE ( 'NONE', #11734, #3805 ) ;
#20132 = ORIENTED_EDGE ( 'NONE', *, *, #11482, .T. ) ;
#20133 = CARTESIAN_POINT ( 'NONE',  ( -145.2889157411863437, -190.4391397928654612, 58.16351966513671812 ) ) ;
#20134 = CARTESIAN_POINT ( 'NONE',  ( 8.869018199820361659, 117.4101421016551967, 9.005765870029716069 ) ) ;
#20135 = CARTESIAN_POINT ( 'NONE',  ( 62.38089001705685632, 99.52138843117178624, -6.434471705120163421 ) ) ;
#20136 = LINE ( 'NONE', #9995, #13941 ) ;
#20137 = ORIENTED_EDGE ( 'NONE', *, *, #14198, .F. ) ;
#20138 = CARTESIAN_POINT ( 'NONE',  ( 38.58424406990784661, 147.5297705074273154, 35.64915139335016647 ) ) ;
#20139 = EDGE_CURVE ( 'NONE', #4691, #14439, #20668, .T. ) ;
#20140 = VECTOR ( 'NONE', #1768, 1000.000000000000000 ) ;
#20142 = EDGE_CURVE ( 'NONE', #495, #5452, #5426, .T. ) ;
#20141 = DIRECTION ( 'NONE',  ( 1.000000000000000000, 0.000000000000000000, 0.000000000000000000 ) ) ;
#20143 = AXIS2_PLACEMENT_3D ( 'NONE', #11748, #16924, #6913 ) ;
#20144 = CARTESIAN_POINT ( 'NONE',  ( 38.01140435219952707, 111.7104996726487514, 34.21067981925357060 ) ) ;
#20145 = CARTESIAN_POINT ( 'NONE',  ( 46.59305225739526435, 61.31518717409399954, 36.81289934271958941 ) ) ;
#20146 = DIRECTION ( 'NONE',  ( 0.000000000000000000, 0.000000000000000000, 1.000000000000000000 ) ) ;
#20147 = CARTESIAN_POINT ( 'NONE',  ( -148.5561028927606344, -162.9938272943107336, 58.62277379824867296 ) ) ;
#20148 = CARTESIAN_POINT ( 'NONE',  ( 38.96631938032478359, 122.4844580088725934, 31.27175355779120025 ) ) ;
#20149 = CARTESIAN_POINT ( 'NONE',  ( -161.4692556286853176, -169.5630981290893260, 49.65701158161630957 ) ) ;
#20150 = CARTESIAN_POINT ( 'NONE',  ( 43.01140435219951996, 10.71049967264875491, 34.21067981925357060 ) ) ;
#20151 = CARTESIAN_POINT ( 'NONE',  ( 46.10157429594899270, 153.8344580088725877, 38.46393386101376421 ) ) ;
#20152 = CARTESIAN_POINT ( 'NONE',  ( 38.58424406990784661, 123.2297705074273040, 32.77220824515698183 ) ) ;
#20153 = CARTESIAN_POINT ( 'NONE',  ( 13.60337824163328513, 137.5875211305428252, 8.692014997358331385 ) ) ;
#20154 = CARTESIAN_POINT ( 'NONE',  ( 43.01140435219951286, 115.4604996726487229, 39.21067981925356349 ) ) ;
#20155 = CARTESIAN_POINT ( 'NONE',  ( 45.74753988029934249, 119.0651871740939924, 30.44471234641812174 ) ) ;
#20156 = CARTESIAN_POINT ( 'NONE',  ( -151.4692556286852891, -196.9891397928655010, 39.65701158161630246 ) ) ;
#20157 = VECTOR ( 'NONE', #14203, 1000.000000000000114 ) ;
#20159 = DIRECTION ( 'NONE',  ( 0.000000000000000000, 1.000000000000000000, 0.000000000000000000 ) ) ;
#20158 = AXIS2_PLACEMENT_3D ( 'NONE', #2199, #14089, #10478 ) ;
#20160 = CARTESIAN_POINT ( 'NONE',  ( 72.81290617574171620, 103.2231620977376281, 0.1530188383368442095 ) ) ;
#20161 = CARTESIAN_POINT ( 'NONE',  ( 50.11350838007777497, 92.61696660072725251, -6.867350599827054758 ) ) ;
#20162 = DIRECTION ( 'NONE',  ( -0.000000000000000000, 1.000000000000000000, -0.000000000000000000 ) ) ;
#20163 = EDGE_CURVE ( 'NONE', #15137, #21430, #13803, .T. ) ;
#20164 = CARTESIAN_POINT ( 'NONE',  ( 38.58424406990785371, 90.52977050742731535, 35.64915139335015937 ) ) ;
#20165 = ORIENTED_EDGE ( 'NONE', *, *, #20255, .F. ) ;
#20166 = ADVANCED_FACE ( 'NONE', ( #12996 ), #12773, .F. ) ;
#20167 = CARTESIAN_POINT ( 'NONE',  ( 121.4021762516569964, 137.5714195593754710, -35.00000000000000000 ) ) ;
#20168 = VERTEX_POINT ( 'NONE', #984 ) ;
#20169 = CARTESIAN_POINT ( 'NONE',  ( 44.55648932407425633, 76.88445800887257064, 29.45539723777780239 ) ) ;
#20170 = LINE ( 'NONE', #16838, #2427 ) ;
#20171 = CARTESIAN_POINT ( 'NONE',  ( 47.05648932407426344, 136.9104996726487400, 37.14960608071593384 ) ) ;
#20173 = CARTESIAN_POINT ( 'NONE',  ( 64.37283757718545019, 93.25908544850187809, -13.41832554473225692 ) ) ;
#20172 = CARTESIAN_POINT ( 'NONE',  ( 46.59305225739526435, 94.31518717409399244, 36.81289934271958941 ) ) ;
#20174 = CARTESIAN_POINT ( 'NONE',  ( -142.0420953463935803, -156.5084106276439968, 46.59394152635518793 ) ) ;
#20175 = CARTESIAN_POINT ( 'NONE',  ( -159.0959885057557983, -193.5938272943107279, 55.19815736654470584 ) ) ;
#20176 = PLANE ( 'NONE',  #10435 ) ;
#20177 = CARTESIAN_POINT ( 'NONE',  ( -143.3790856849358306, -177.3630981290893089, 55.53486410454105027 ) ) ;
#20178 = CARTESIAN_POINT ( 'NONE',  ( 116.4417310231185780, -126.9891397928655010, 19.99999999999999645 ) ) ;
#20179 = CARTESIAN_POINT ( 'NONE',  ( 47.43856463449117200, 152.0297705074273438, 32.77220824515698183 ) ) ;
#20180 = DIRECTION ( 'NONE',  ( 0.000000000000000000, -1.000000000000000000, 0.000000000000000000 ) ) ;
#20181 = CARTESIAN_POINT ( 'NONE',  ( 66.24914683137549787, 94.76885710642066840, 6.506024766557033878 ) ) ;
#20182 = CARTESIAN_POINT ( 'NONE',  ( 43.01140435219951286, 146.3651871740939896, 29.55568802177586107 ) ) ;
#20183 = CARTESIAN_POINT ( 'NONE',  ( -160.8964159109769696, -160.8938272943107393, 49.65701158161630957 ) ) ;
#20184 = CARTESIAN_POINT ( 'NONE',  ( -143.8425227516148084, -171.9584106276440423, 55.19815736654470584 ) ) ;
#20185 = ORIENTED_EDGE ( 'NONE', *, *, #16291, .F. ) ;
#20186 = CARTESIAN_POINT ( 'NONE',  ( 41.64333658814960870, 60.71518717409399102, 38.42115945441014446 ) ) ;
#20187 = CARTESIAN_POINT ( 'NONE',  ( -145.6429501568359797, -162.2084106276440707, 41.63779006702063867 ) ) ;
#20188 = CARTESIAN_POINT ( 'NONE',  ( 32.55111017628423298, 93.63144033427927582, -0.1575420629755377999 ) ) ;
#20189 = CARTESIAN_POINT ( 'NONE',  ( 39.42975644700377558, 120.4151871740940010, 36.81289934271958941 ) ) ;
#20190 = ORIENTED_EDGE ( 'NONE', *, *, #21595, .T. ) ;
#20191 = ORIENTED_EDGE ( 'NONE', *, *, #14609, .T. ) ;
#20192 = CARTESIAN_POINT ( 'NONE',  ( 41.46631938032478359, 147.3844580088725991, 38.96596240072933170 ) ) ;
#20193 = VERTEX_POINT ( 'NONE', #6375 ) ;
#20194 = CARTESIAN_POINT ( 'NONE',  ( 38.96631938032478359, 99.08445800887258770, 37.14960608071593384 ) ) ;
#20195 = CARTESIAN_POINT ( 'NONE',  ( 46.59305225739526435, 154.5797705074273267, 36.81289934271958941 ) ) ;
#20196 = CARTESIAN_POINT ( 'NONE',  ( 44.37947211624943833, 67.27977050742731535, 38.42115945441014446 ) ) ;
#20198 = CARTESIAN_POINT ( 'NONE',  ( 67.71458430423905384, 106.3058120325361671, 6.227933542621733487 ) ) ;
#20197 = CARTESIAN_POINT ( 'NONE',  ( 39.42975644700377558, 125.8151871740940067, 31.60846029578754468 ) ) ;
#20199 = CARTESIAN_POINT ( 'NONE',  ( 43.01140435219951286, 82.46049967264873715, 39.46799094044489209 ) ) ;
#20200 = CARTESIAN_POINT ( 'NONE',  ( 9.203281625063985061, 114.5318647093721864, 15.91056058043385413 ) ) ;
#20201 = CARTESIAN_POINT ( 'NONE',  ( 43.80332655382222384, 97.53738109496902098, 39.21067981925354928 ) ) ;
#20202 = DIRECTION ( 'NONE',  ( 0.000000000000000000, 0.000000000000000000, 1.000000000000000000 ) ) ;
#20203 = CARTESIAN_POINT ( 'NONE',  ( 41.64333658814960870, 77.51518717409399528, 30.00020018409699318 ) ) ;
#20204 = CARTESIAN_POINT ( 'NONE',  ( 39.96131221638199804, 144.7218222453713565, 38.18604851697274682 ) ) ;
#20205 = CARTESIAN_POINT ( 'NONE',  ( 39.92123440845005433, 133.1604996726487684, 38.46393386101375711 ) ) ;
#20206 = VERTEX_POINT ( 'NONE', #9697 ) ;
#20207 = CARTESIAN_POINT ( 'NONE',  ( 38.58424406990784661, 63.52977050742730825, 35.64915139335016647 ) ) ;
#20208 = CARTESIAN_POINT ( 'NONE',  ( -148.5561028927606344, -183.0584106276440650, 40.69124936498395328 ) ) ;
#20209 = CARTESIAN_POINT ( 'NONE',  ( 68.80033453084351436, 142.5431462587704061, -3.212652714419679700 ) ) ;
#20210 = EDGE_CURVE ( 'NONE', #13608, #12008, #9912, .T. ) ;
#20211 = CARTESIAN_POINT ( 'NONE',  ( -143.8425227516148084, -174.9584106276440707, 55.19815736654470584 ) ) ;
#20212 = VERTEX_POINT ( 'NONE', #12884 ) ;
#20213 = CARTESIAN_POINT ( 'NONE',  ( 39.42975644700377558, 152.8151871740940067, 31.60846029578754468 ) ) ;
#20214 = DIRECTION ( 'NONE',  ( -1.186952418100008983E-16, -0.000000000000000000, -1.000000000000000000 ) ) ;
#20215 = CARTESIAN_POINT ( 'NONE',  ( 40.27526882409969744, 117.8297705074273551, 37.97664729208901235 ) ) ;
#20216 = CARTESIAN_POINT ( 'NONE',  ( 51.60797029699607918, 86.77139250312444574, -6.946567135388369785 ) ) ;
#20217 = ORIENTED_EDGE ( 'NONE', *, *, #7944, .T. ) ;
#20218 = CARTESIAN_POINT ( 'NONE',  ( 55.29376081731632553, 145.2908078538121401, -2.581636314160848489 ) ) ;
#20219 = ORIENTED_EDGE ( 'NONE', *, *, #5810, .T. ) ;
#20220 = CARTESIAN_POINT ( 'NONE',  ( 43.01140435219951286, 118.1297705074273097, 38.86567161673127657 ) ) ;
#20221 = CARTESIAN_POINT ( 'NONE',  ( 38.96631938032478359, 126.4104996726487542, 31.27175355779120025 ) ) ;
#20222 = CARTESIAN_POINT ( 'NONE',  ( 46.59305225739526435, 157.9151871740940010, 31.60846029578754468 ) ) ;
#20223 =( BOUNDED_CURVE ( )  B_SPLINE_CURVE ( 2, ( #3036, #9774, #20452, #18580, #4914, #13291, #13507, #15271, #1719, #18470, #279, #8772, #15046 ),
 .UNSPECIFIED., .F., .F. ) 
 B_SPLINE_CURVE_WITH_KNOTS ( ( 3, 2, 2, 2, 2, 2, 3 ),
 ( 0.1985294117647058709, 0.2000000000000000111, 0.2029411764705882359, 0.2058823529411764608, 0.2088235294117647134, 0.2117647058823529382, 0.2132352941176470507 ),
 .UNSPECIFIED. ) 
 CURVE ( )  GEOMETRIC_REPRESENTATION_ITEM ( )  RATIONAL_B_SPLINE_CURVE ( ( 0.9755282581475765991, 0.9755282581475764880, 1.000000000000000000, 0.9510565162951535312, 1.000000000000000000, 0.9510565162951535312, 1.000000000000000000, 0.9510565162951535312, 1.000000000000000000, 0.9510565162951535312, 1.000000000000000000, 0.9755282581475768211, 0.9755282581475768211 ) ) 
 REPRESENTATION_ITEM ( '' )  );
#20224 = ADVANCED_FACE ( 'NONE', ( #1307 ), #4831, .F. ) ;
#20225 = CARTESIAN_POINT ( 'NONE',  ( 74.11624783127615501, 105.8034190341144978, 7.057826790323951549 ) ) ;
#20226 = CARTESIAN_POINT ( 'NONE',  ( -143.9637021292201950, -126.9891397928655010, 62.65701158161630957 ) ) ;
#20227 = CARTESIAN_POINT ( 'NONE',  ( 132.3486983259487886, 110.2203079035327420, -25.00000000000000000 ) ) ;
#20228 = CARTESIAN_POINT ( 'NONE',  ( -145.2889157411863721, -181.4391397928654612, 58.16351966513671812 ) ) ;
#20229 = DIRECTION ( 'NONE',  ( 1.000000000000000000, 0.000000000000000000, -0.000000000000000000 ) ) ;
#20230 = CARTESIAN_POINT ( 'NONE',  ( 46.10157429594899270, 76.76049967264872009, 38.46393386101375711 ) ) ;
#20231 = ITEM_DEFINED_TRANSFORMATION ( 'NONE', 'NONE', #17940,  #12657 ) ;
#20232 = CARTESIAN_POINT ( 'NONE',  ( 41.46631938032478359, 98.18445800887256780, 29.45539723777780239 ) ) ;
#20233 = CARTESIAN_POINT ( 'NONE',  ( 40.27526882409969033, 89.92977050742730682, 30.44471234641811819 ) ) ;
#20234 = CARTESIAN_POINT ( 'NONE',  ( 52.49585387951581339, 146.4637788833130685, -2.700609006624497876 ) ) ;
#20235 = CARTESIAN_POINT ( 'NONE',  ( -160.8964159109769696, -169.7438272943106767, 52.72008163687743121 ) ) ;
#20236 = VECTOR ( 'NONE', #2856, 1000.000000000000000 ) ;
#20237 = CARTESIAN_POINT ( 'NONE',  ( 46.59305225739526435, 88.91518717409400097, 31.60846029578754468 ) ) ;
#20238 = FACE_OUTER_BOUND ( 'NONE', #13074, .T. ) ;
#20239 = VERTEX_POINT ( 'NONE', #3069 ) ;
#20240 = DIRECTION ( 'NONE',  ( -0.000000000000000000, -0.000000000000000000, 1.000000000000000000 ) ) ;
#20241 = AXIS2_PLACEMENT_3D ( 'NONE', #16170, #2731, #12655 ) ;
#20242 = CARTESIAN_POINT ( 'NONE',  ( 17.14282613681034917, 97.48634091255654255, 8.291567264837656381 ) ) ;
#20243 = CARTESIAN_POINT ( 'NONE',  ( 40.27526882409969744, 138.8297705074272983, 37.97664729208901235 ) ) ;
#20244 = CARTESIAN_POINT ( 'NONE',  ( 19.79626631456835284, 104.0394230781280669, 2.494070082984220171 ) ) ;
#20245 = EDGE_CURVE ( 'NONE', #2574, #6176, #6684, .T. ) ;
#20246 = CARTESIAN_POINT ( 'NONE',  ( 44.82204965540741171, 59.43124467221783647, 30.14400234367970910 ) ) ;
#20247 = VERTEX_POINT ( 'NONE', #16182 ) ;
#20248 = CARTESIAN_POINT ( 'NONE',  ( 46.59305225739526435, 145.5797705074273267, 36.81289934271958941 ) ) ;
#20249 = CARTESIAN_POINT ( 'NONE',  ( 47.05648932407426344, 152.5104996726487343, 31.27175355779120025 ) ) ;
#20250 = CARTESIAN_POINT ( 'NONE',  ( 43.01140435219951996, 10.71049967264875491, 29.21067981925357060 ) ) ;
#20251 = CARTESIAN_POINT ( 'NONE',  ( -161.4692556286852891, -169.4130981290893203, 52.90620854394536821 ) ) ;
#20252 = CARTESIAN_POINT ( 'NONE',  ( -145.2889157411863437, -173.6130981290893089, 41.15050349809589392 ) ) ;
#20253 = LINE ( 'NONE', #2161, #2994 ) ;
#20254 = CARTESIAN_POINT ( 'NONE',  ( -145.2889157411863721, -170.6130981290892805, 41.15050349809590102 ) ) ;
#20255 = EDGE_CURVE ( 'NONE', #5452, #6422, #5583, .T. ) ;
#20256 = CARTESIAN_POINT ( 'NONE',  ( 38.01140435219952707, 143.7844580088725763, 34.21067981925357060 ) ) ;
#20257 = CARTESIAN_POINT ( 'NONE',  ( 40.27526882409969033, 119.9297705074272926, 30.44471234641811819 ) ) ;
#20258 = CARTESIAN_POINT ( 'NONE',  ( 44.40591325931411859, 91.66001841764941105, -0.6336051400208910778 ) ) ;
#20259 = CARTESIAN_POINT ( 'NONE',  ( 48.01140435219951996, 100.2844580088725905, 34.21067981925357060 ) ) ;
#20260 = CARTESIAN_POINT ( 'NONE',  ( 43.01140435219951286, 114.8651871740939896, 38.86567161673127657 ) ) ;
#20261 = CARTESIAN_POINT ( 'NONE',  ( 43.01140435219951286, 126.5344580088725621, 39.21067981925356349 ) ) ;
#20262 = CARTESIAN_POINT ( 'NONE',  ( 58.73109577922829061, 150.2274887891485662, -1.632724326791204605 ) ) ;
#20263 = ADVANCED_FACE ( 'NONE', ( #4608 ), #17938, .T. ) ;
#20264 = CARTESIAN_POINT ( 'NONE',  ( 15.50679444821833819, 113.6848169819070193, -5.081469017220888063 ) ) ;
#20265 = CARTESIAN_POINT ( 'NONE',  ( -143.3790856849358306, -185.7630981290893146, 43.77915905869157598 ) ) ;
#20266 = CARTESIAN_POINT ( 'NONE',  ( 41.64333658814960870, 81.97977050742731819, 38.42115945441014446 ) ) ;
#20267 = EDGE_LOOP ( 'NONE', ( #12716, #12421, #5722, #17750 ) ) ;
#20268 = AXIS2_PLACEMENT_3D ( 'NONE', #8363, #21810, #6719 ) ;
#20269 = PLANE ( 'NONE',  #11173 ) ;
#20270 = CARTESIAN_POINT ( 'NONE',  ( 48.01140435219951996, 73.28445800887257633, 34.21067981925357060 ) ) ;
#20271 = CARTESIAN_POINT ( 'NONE',  ( 38.01140435219952707, 59.78445800887258343, 34.21067981925357060 ) ) ;
#20272 = CARTESIAN_POINT ( 'NONE',  ( 44.55648932407425633, 130.6104996726487286, 38.96596240072933170 ) ) ;
#20274 = CARTESIAN_POINT ( 'NONE',  ( 77.08865571979157494, 122.1823731668103221, -14.48986716664726870 ) ) ;
#20273 = CARTESIAN_POINT ( 'NONE',  ( 47.43856463449117200, 91.46518717409398391, 35.64915139335016647 ) ) ;
#20275 = CARTESIAN_POINT ( 'NONE',  ( -143.8425227516148084, -159.9584106276440423, 55.19815736654470584 ) ) ;
#20276 = CARTESIAN_POINT ( 'NONE',  ( -160.8964159109769696, -190.8938272943107393, 49.65701158161630957 ) ) ;
#20277 = CARTESIAN_POINT ( 'NONE',  ( 43.01140435219951996, 10.71049967264875491, 34.21067981925357060 ) ) ;
#20278 = EDGE_CURVE ( 'NONE', #4745, #13613, #18629, .T. ) ;
#20279 = CARTESIAN_POINT ( 'NONE',  ( -148.3790856849358306, -177.6630981290893203, 59.16757674456786020 ) ) ;
#20280 = CYLINDRICAL_SURFACE ( 'NONE', #11856, 10.00000000000000888 ) ;
#20281 = CARTESIAN_POINT ( 'NONE',  ( 47.43856463449118621, 148.8797705074273097, 34.21067981925357060 ) ) ;
#20282 = DIRECTION ( 'NONE',  ( 0.000000000000000000, 1.000000000000000000, 0.000000000000000000 ) ) ;
#20283 = CARTESIAN_POINT ( 'NONE',  ( 70.26356658872128946, 140.6255928306487704, 11.86290872716119615 ) ) ;
#20284 = CARTESIAN_POINT ( 'NONE',  ( 38.58424406990785371, 150.2651871740940237, 35.64915139335015937 ) ) ;
#20285 = CIRCLE ( 'NONE', #18858, 21.90454335994854063 ) ;
#20286 = CARTESIAN_POINT ( 'NONE',  ( -160.8964159109769696, -163.8938272943107393, 49.65701158161630957 ) ) ;
#20287 = CARTESIAN_POINT ( 'NONE',  ( -142.0420953463935803, -174.5084106276440252, 46.59394152635518083 ) ) ;
#20288 = LINE ( 'NONE', #4177, #9578 ) ;
#20289 = CARTESIAN_POINT ( 'NONE',  ( -143.8425227516148084, -162.9584106276440423, 55.19815736654470584 ) ) ;
#20290 = CARTESIAN_POINT ( 'NONE',  ( 51.76721073900363734, 146.7980033588722506, -3.728880589165500137 ) ) ;
#20291 = CARTESIAN_POINT ( 'NONE',  ( 40.27526882409969033, 128.6651871740940010, 30.44471234641811819 ) ) ;
#20292 = VERTEX_POINT ( 'NONE', #1420 ) ;
#20293 = VERTEX_POINT ( 'NONE', #11437 ) ;
#20294 = CARTESIAN_POINT ( 'NONE',  ( 185.6125732647967368, 204.7716666330005921, 23.27362312593913174 ) ) ;
#20295 = ORIENTED_EDGE ( 'NONE', *, *, #21194, .T. ) ;
#20296 = CARTESIAN_POINT ( 'NONE',  ( 38.96631938032478359, 98.48445800887257917, 31.27175355779120025 ) ) ;
#20297 = CARTESIAN_POINT ( 'NONE',  ( 43.80332655382220253, 115.5373810949689926, 39.21067981925355639 ) ) ;
#20298 = CARTESIAN_POINT ( 'NONE',  ( 47.43856463449117200, 65.02977050742732956, 32.77220824515698183 ) ) ;
#20300 = CARTESIAN_POINT ( 'NONE',  ( 57.54249972904700172, 143.9818934734506115, -15.48196187774845356 ) ) ;
#20299 = CARTESIAN_POINT ( 'NONE',  ( 47.43856463449117200, 118.4651871740939981, 35.64915139335016647 ) ) ;
#20301 = AXIS2_PLACEMENT_3D ( 'NONE', #20753, #12365, #19103 ) ;
#20302 = CARTESIAN_POINT ( 'NONE',  ( 41.46631938032478359, 81.11049967264874283, 29.45539723777780239 ) ) ;
#20303 = CARTESIAN_POINT ( 'NONE',  ( 44.55648932407425633, 148.8844580088725991, 29.45539723777780239 ) ) ;
#20304 = EDGE_CURVE ( 'NONE', #6019, #14386, #6296, .T. ) ;
#20305 = CARTESIAN_POINT ( 'NONE',  ( 48.01140435219951996, 98.36049967264872862, 32.58608133808903773 ) ) ;
#20306 = CARTESIAN_POINT ( 'NONE',  ( -151.4692556286852891, -136.9891397928655010, -54.65701158161630246 ) ) ;
#20307 = CARTESIAN_POINT ( 'NONE',  ( 40.27526882409969033, 75.56518717409399244, 37.97664729208901946 ) ) ;
#20308 = CYLINDRICAL_SURFACE ( 'NONE', #13638, 4.999999999999997335 ) ;
#20309 = CARTESIAN_POINT ( 'NONE',  ( 38.01140435219952707, 122.7844580088725763, 34.21067981925357060 ) ) ;
#20310 = CYLINDRICAL_SURFACE ( 'NONE', #6047, 10.00000000000000888 ) ;
#20311 = EDGE_LOOP ( 'NONE', ( #6878, #6799, #7121, #14901 ) ) ;
#20312 = CARTESIAN_POINT ( 'NONE',  ( 38.58424406990784661, 69.22977050742731819, 32.77220824515698183 ) ) ;
#20313 = CARTESIAN_POINT ( 'NONE',  ( -157.2955611005346270, -188.6084106276440764, 41.63779006702063867 ) ) ;
#20314 = AXIS2_PLACEMENT_3D ( 'NONE', #20844, #9493, #5736 ) ;
#20315 = CARTESIAN_POINT ( 'NONE',  ( 76.33227852969314142, 111.7084249013780806, -2.141487123205697340 ) ) ;
#20316 = CARTESIAN_POINT ( 'NONE',  ( -160.8964159109769696, -176.0084106276440536, 52.72008163687743121 ) ) ;
#20317 = ORIENTED_EDGE ( 'NONE', *, *, #7587, .F. ) ;
#20318 = CARTESIAN_POINT ( 'NONE',  ( 47.43856463449117200, 151.4651871740939839, 35.64915139335016647 ) ) ;
#20319 = DIRECTION ( 'NONE',  ( 0.000000000000000000, -0.000000000000000000, -1.000000000000000000 ) ) ;
#20320 = CARTESIAN_POINT ( 'NONE',  ( 46.59305225739526435, 116.1797705074273210, 31.60846029578754468 ) ) ;
#20321 = CARTESIAN_POINT ( 'NONE',  ( 57.78275410301085913, 89.02518083909171764, -0.1607367497116551913 ) ) ;
#20322 = VERTEX_POINT ( 'NONE', #3183 ) ;
#20323 = EDGE_CURVE ( 'NONE', #20292, #11247, #12283, .T. ) ;
#20324 = CARTESIAN_POINT ( 'NONE',  ( 69.04633063039527485, 130.7408809369782716, -8.772150750671475095 ) ) ;
#20325 = ORIENTED_EDGE ( 'NONE', *, *, #11916, .T. ) ;
#20326 = CARTESIAN_POINT ( 'NONE',  ( 41.64333658814960870, 111.9797705074273324, 38.42115945441014446 ) ) ;
#20327 = DIRECTION ( 'NONE',  ( 0.000000000000000000, 1.000000000000000000, 0.000000000000000000 ) ) ;
#20328 = CARTESIAN_POINT ( 'NONE',  ( 79.42064422693164261, 282.0082918409407284, -4.000000000000002665 ) ) ;
#20329 = CARTESIAN_POINT ( 'NONE',  ( 46.59305225739526435, 151.9151871740940010, 31.60846029578754468 ) ) ;
#20330 = VECTOR ( 'NONE', #20519, 1000.000000000000000 ) ;
#20331 = CARTESIAN_POINT ( 'NONE',  ( 45.50561661668613311, 153.9697812235645245, 4.915054502968218664 ) ) ;
#20332 = CARTESIAN_POINT ( 'NONE',  ( 38.58424406990786082, 159.1151871740940180, 34.21067981925357060 ) ) ;
#20333 = DIRECTION ( 'NONE',  ( -0.000000000000000000, 1.000000000000000000, -0.000000000000000000 ) ) ;
#20334 = CARTESIAN_POINT ( 'NONE',  ( -157.6495955161842062, -179.9391397928654328, 41.15050349809590102 ) ) ;
#20335 = CARTESIAN_POINT ( 'NONE',  ( -153.0531000319306827, -182.2362167067690564, 39.65701158161630957 ) ) ;
#20336 = UNCERTAINTY_MEASURE_WITH_UNIT (LENGTH_MEASURE( 1.000000000000000082E-05 ), #21579, 'distance_accuracy_value', 'NONE');
#20337 = DIRECTION ( 'NONE',  ( 1.000000000000000000, 0.000000000000000000, 0.000000000000000000 ) ) ;
#20338 = CARTESIAN_POINT ( 'NONE',  ( 48.01140435219951996, 97.13445800887257064, 35.83527830041809636 ) ) ;
#20339 = CARTESIAN_POINT ( 'NONE',  ( 46.59305225739526435, 92.17977050742732104, 31.60846029578754468 ) ) ;
#20340 = CARTESIAN_POINT ( 'NONE',  ( 29.22050282933603071, 144.5044581412665536, -3.652897588741476742 ) ) ;
#20341 = CARTESIAN_POINT ( 'NONE',  ( -151.4692556286852891, -172.1438272943107108, 59.56931450028537967 ) ) ;
#20342 = CARTESIAN_POINT ( 'NONE',  ( 47.43856463449118621, 76.61518717409400381, 34.21067981925357060 ) ) ;
#20344 = CIRCLE ( 'NONE', #10837, 5.000000000000004441 ) ;
#20343 = CARTESIAN_POINT ( 'NONE',  ( -151.4692556286852607, -171.2391397928654726, 39.65701158161629536 ) ) ;
#20345 = FACE_OUTER_BOUND ( 'NONE', #12556, .T. ) ;
#20346 = ORIENTED_EDGE ( 'NONE', *, *, #14052, .F. ) ;
#20347 = PLANE ( 'NONE',  #17139 ) ;
#20348 = FACE_OUTER_BOUND ( 'NONE', #13149, .T. ) ;
#20349 = CARTESIAN_POINT ( 'NONE',  ( 67.81612255856859406, 106.6615363072494915, -6.791355845220972576 ) ) ;
#20350 = DIRECTION ( 'NONE',  ( 0.000000000000000000, 1.000000000000000000, 0.000000000000000000 ) ) ;
#20351 =( BOUNDED_CURVE ( )  B_SPLINE_CURVE ( 2, ( #4483, #9354, #10793, #19164, #756, #11001, #21043, #12871, #1082, #9471, #17711, #9145, #14624 ),
 .UNSPECIFIED., .F., .F. ) 
 B_SPLINE_CURVE_WITH_KNOTS ( ( 3, 2, 2, 2, 2, 2, 3 ),
 ( 0.8750000000000000000, 0.8764705882352941124, 0.8794117647058823373, 0.8823529411764705621, 0.8852941176470587870, 0.8882352941176470118, 0.8897058823529412352 ),
 .UNSPECIFIED. ) 
 CURVE ( )  GEOMETRIC_REPRESENTATION_ITEM ( )  RATIONAL_B_SPLINE_CURVE ( ( 0.9755282581475768211, 0.9755282581475768211, 1.000000000000000000, 0.9510565162951535312, 1.000000000000000000, 0.9510565162951535312, 1.000000000000000000, 0.9510565162951535312, 1.000000000000000000, 0.9510565162951535312, 1.000000000000000000, 0.9755282581475758219, 0.9755282581475768211 ) ) 
 REPRESENTATION_ITEM ( '' )  );
#20352 = ORIENTED_EDGE ( 'NONE', *, *, #5164, .T. ) ;
#20353 = CARTESIAN_POINT ( 'NONE',  ( 47.43856463449118621, 139.8797705074273381, 34.21067981925357060 ) ) ;
#20354 = CARTESIAN_POINT ( 'NONE',  ( 41.64333658814960870, 99.97977050742731819, 38.42115945441014446 ) ) ;
#20355 = CARTESIAN_POINT ( 'NONE',  ( 38.01140435219952707, 141.7104996726487514, 34.21067981925357060 ) ) ;
#20356 = CARTESIAN_POINT ( 'NONE',  ( 45.74753988029933538, 62.06518717409399244, 30.44471234641811819 ) ) ;
#20357 = DIRECTION ( 'NONE',  ( -0.000000000000000000, -0.000000000000000000, -1.000000000000000000 ) ) ;
#20358 = DIRECTION ( 'NONE',  ( 0.000000000000000000, 0.000000000000000000, 1.000000000000000000 ) ) ;
#20359 = LINE ( 'NONE', #8898, #13205 ) ;
#20360 = CARTESIAN_POINT ( 'NONE',  ( -141.4692556286852891, -164.9130981290892919, 46.40781461928724383 ) ) ;
#20361 =( GEOMETRIC_REPRESENTATION_CONTEXT ( 3 ) GLOBAL_UNCERTAINTY_ASSIGNED_CONTEXT ( ( #7539 ) ) GLOBAL_UNIT_ASSIGNED_CONTEXT ( ( #5118, #9270, #11126 ) ) REPRESENTATION_CONTEXT ( 'NONE', 'WORKASPACE' ) );
#20362 = DIRECTION ( 'NONE',  ( 0.000000000000000000, 0.000000000000000000, -1.000000000000000000 ) ) ;
#20363 = CARTESIAN_POINT ( 'NONE',  ( 48.01140435219951996, 139.2844580088725763, 34.21067981925357060 ) ) ;
#20364 = CARTESIAN_POINT ( 'NONE',  ( 38.58424406990786082, 126.3797705074273239, 34.21067981925357060 ) ) ;
#20365 = CARTESIAN_POINT ( 'NONE',  ( 59.79647059797250819, 142.6686746773435459, -3.371582063846674693 ) ) ;
#20366 = FACE_OUTER_BOUND ( 'NONE', #6959, .T. ) ;
#20367 = CARTESIAN_POINT ( 'NONE',  ( 38.58424406990785371, 108.2651871740939811, 35.64915139335015937 ) ) ;
#20368 = CARTESIAN_POINT ( 'NONE',  ( 41.46631938032478359, 125.1844580088725678, 29.45539723777780239 ) ) ;
#20369 = CARTESIAN_POINT ( 'NONE',  ( 11.06625761453251933, 131.9899775861109106, 3.486483074593720755 ) ) ;
#20370 = CARTESIAN_POINT ( 'NONE',  ( 71.16904767199986281, 118.3707548728134213, -1.272037577920760665 ) ) ;
#20371 = ADVANCED_FACE ( 'NONE', ( #11119 ), #16290, .T. ) ;
#20372 = CARTESIAN_POINT ( 'NONE',  ( 41.64333658814960870, 89.77977050742731535, 30.00020018409699318 ) ) ;
#20373 = EDGE_CURVE ( 'NONE', #19098, #3809, #1197, .T. ) ;
#20374 = EDGE_LOOP ( 'NONE', ( #21432, #19714, #9721, #10065 ) ) ;
#20375 = CARTESIAN_POINT ( 'NONE',  ( 46.10157429594899270, 133.7604996726487059, 38.46393386101375711 ) ) ;
#20376 = CARTESIAN_POINT ( 'NONE',  ( 38.01140435219952707, 68.78445800887257633, 34.21067981925357060 ) ) ;
#20377 = CARTESIAN_POINT ( 'NONE',  ( 131.8222645499855901, 267.5435007770738025, -6.999999999999995559 ) ) ;
#20378 = CARTESIAN_POINT ( 'NONE',  ( 48.01140435219951996, 131.3604996726487002, 32.58608133808903773 ) ) ;
#20380 = CARTESIAN_POINT ( 'NONE',  ( 8.857566569312460558, 119.8222194325741725, -10.91815776494309098 ) ) ;
#20379 = CARTESIAN_POINT ( 'NONE',  ( 43.01140435219951286, 83.36518717409397539, 29.55568802177586463 ) ) ;
#20381 = CARTESIAN_POINT ( 'NONE',  ( -142.0420953463935803, -162.5084106276440536, 46.59394152635518793 ) ) ;
#20382 = CARTESIAN_POINT ( 'NONE',  ( -160.8964159109769696, -181.7438272943107336, 52.72008163687743121 ) ) ;
#20383 = LINE ( 'NONE', #13542, #8328 ) ;
#20384 = CARTESIAN_POINT ( 'NONE',  ( -159.5594255724347761, -193.8630981290893089, 43.77915905869157598 ) ) ;
#20385 = CARTESIAN_POINT ( 'NONE',  ( 147.5268905834513475, 193.0332408774651185, -50.99999999999998579 ) ) ;
#20386 = CARTESIAN_POINT ( 'NONE',  ( -161.4692556286852891, -173.6391397928654499, 46.40781461928724383 ) ) ;
#20387 = CARTESIAN_POINT ( 'NONE',  ( 44.37947211624943833, 155.4797705074273324, 30.00020018409699318 ) ) ;
#20388 = CARTESIAN_POINT ( 'NONE',  ( 47.43856463449118621, 103.8797705074273239, 34.21067981925357060 ) ) ;
#20389 = CARTESIAN_POINT ( 'NONE',  ( 53.04203944364535772, 87.17698241397053494, 14.00585298808814194 ) ) ;
#20390 = CARTESIAN_POINT ( 'NONE',  ( 44.37947211624943833, 142.0151871740939953, 38.42115945441014446 ) ) ;
#20391 = CARTESIAN_POINT ( 'NONE',  ( 46.10157429594899270, 66.83445800887258770, 38.46393386101375711 ) ) ;
#20392 = CARTESIAN_POINT ( 'NONE',  ( -159.0959885057557983, -175.8584106276440480, 55.19815736654470584 ) ) ;
#20393 = VECTOR ( 'NONE', #17265, 1000.000000000000114 ) ;
#20394 = CARTESIAN_POINT ( 'NONE',  ( 44.37947211624943833, 64.01518717409400949, 38.42115945441014446 ) ) ;
#20395 = CARTESIAN_POINT ( 'NONE',  ( -142.0420953463935803, -159.8084106276440934, 52.72008163687743831 ) ) ;
#20396 = CARTESIAN_POINT ( 'NONE',  ( 24.80496442426440140, 98.26638142913259344, 0.1995735771552373528 ) ) ;
#20397 = SURFACE_STYLE_FILL_AREA ( #6956 ) ;
#20398 = CARTESIAN_POINT ( 'NONE',  ( 47.43856463449118621, 115.6151871740940038, 34.21067981925357060 ) ) ;
#20399 = ORIENTED_EDGE ( 'NONE', *, *, #16967, .T. ) ;
#20400 = ORIENTED_EDGE ( 'NONE', *, *, #16894, .F. ) ;
#20401 = ORIENTED_EDGE ( 'NONE', *, *, #3541, .F. ) ;
#20402 = CARTESIAN_POINT ( 'NONE',  ( 48.01140435219951996, 100.2844580088725905, 34.21067981925357060 ) ) ;
#20403 = CARTESIAN_POINT ( 'NONE',  ( 46.59305225739526435, 158.1797705074273210, 31.60846029578754468 ) ) ;
#20404 = EDGE_CURVE ( 'NONE', #2626, #9805, #7826, .T. ) ;
#20405 = CARTESIAN_POINT ( 'NONE',  ( 48.01140435219951996, 158.0604996726486888, 35.83527830041810347 ) ) ;
#20407 = CARTESIAN_POINT ( 'NONE',  ( 30.72731853479779929, 94.52359049060457608, 14.91853181686295038 ) ) ;
#20406 = CARTESIAN_POINT ( 'NONE',  ( 43.01140435219951286, 113.3651871740939754, 29.55568802177586463 ) ) ;
#20408 =( BOUNDED_CURVE ( )  B_SPLINE_CURVE ( 2, ( #14895, #3002, #1024, #21643, #21308, #9522, #7760, #12924, #19649, #14458, #4540, #11260, #2894 ),
 .UNSPECIFIED., .F., .F. ) 
 B_SPLINE_CURVE_WITH_KNOTS ( ( 3, 2, 2, 2, 2, 2, 3 ),
 ( 0.9485294117647058432, 0.9499999999999999556, 0.9529411764705881804, 0.9558823529411765163, 0.9588235294117647411, 0.9617647058823529660, 0.9632352941176470784 ),
 .UNSPECIFIED. ) 
 CURVE ( )  GEOMETRIC_REPRESENTATION_ITEM ( )  RATIONAL_B_SPLINE_CURVE ( ( 0.9755282581475768211, 0.9755282581475768211, 1.000000000000000000, 0.9510565162951535312, 1.000000000000000000, 0.9510565162951535312, 1.000000000000000000, 0.9510565162951535312, 1.000000000000000000, 0.9510565162951535312, 1.000000000000000000, 0.9755282581475768211, 0.9755282581475768211 ) ) 
 REPRESENTATION_ITEM ( '' )  );
#20409 = EDGE_CURVE ( 'NONE', #5965, #1030, #7042, .T. ) ;
#20410 = CARTESIAN_POINT ( 'NONE',  ( 38.01140435219951996, 72.86049967264872862, 35.83527830041810347 ) ) ;
#20411 = CARTESIAN_POINT ( 'NONE',  ( 42.21948215057684450, 74.11133943119283174, 29.21067981925356705 ) ) ;
#20412 = CARTESIAN_POINT ( 'NONE',  ( 41.46631938032478359, 72.38445800887258486, 38.96596240072933170 ) ) ;
#20413 = CARTESIAN_POINT ( 'NONE',  ( 47.75426913703832099, 95.36076719471033414, 35.82660397859488199 ) ) ;
#20414 = CARTESIAN_POINT ( 'NONE',  ( 41.64333658814960870, 75.71518717409401233, 38.42115945441014446 ) ) ;
#20415 = CARTESIAN_POINT ( 'NONE',  ( 136.0032066456581390, 182.5367998656340944, 34.00000000000001421 ) ) ;
#20416 = CARTESIAN_POINT ( 'NONE',  ( -157.2955611005346270, -182.3438272943106995, 41.63779006702063867 ) ) ;
#20417 = CARTESIAN_POINT ( 'NONE',  ( -176.9699209214867608, -136.9891397928655010, 67.64809332337415526 ) ) ;
#20418 = VERTEX_POINT ( 'NONE', #6608 ) ;
#20419 = CARTESIAN_POINT ( 'NONE',  ( -148.5561028927606344, -184.2584106276440536, 58.62277379824867296 ) ) ;
#20420 = CARTESIAN_POINT ( 'NONE',  ( 70.26356658872128946, 140.6255928306487704, 11.86290872716119615 ) ) ;
#20421 = CARTESIAN_POINT ( 'NONE',  ( -154.3824083646099439, -179.7584106276440536, 40.69124936498395328 ) ) ;
#20422 = ORIENTED_EDGE ( 'NONE', *, *, #14698, .T. ) ;
#20423 = CARTESIAN_POINT ( 'NONE',  ( 43.01140435219951286, 155.3651871740939896, 29.55568802177586463 ) ) ;
#20424 = PRODUCT_DEFINITION_FORMATION_WITH_SPECIFIED_SOURCE ( 'ANY', '', #13296, .NOT_KNOWN. ) ;
#20425 = CARTESIAN_POINT ( 'NONE',  ( 44.37947211624943833, 158.2151871740939839, 30.00020018409699318 ) ) ;
#20426 = CARTESIAN_POINT ( 'NONE',  ( 38.58424406990786082, 114.3797705074273097, 34.21067981925357060 ) ) ;
#20427 = CARTESIAN_POINT ( 'NONE',  ( 53.71239221804358976, 87.38980250447106357, 6.982120393166105998 ) ) ;
#20428 = ORIENTED_EDGE ( 'NONE', *, *, #20142, .T. ) ;
#20429 = EDGE_CURVE ( 'NONE', #13745, #19857, #7732, .T. ) ;
#20430 = CARTESIAN_POINT ( 'NONE',  ( 24.78883071187807730, 141.3519591882296709, -10.86778418981948846 ) ) ;
#20431 = ORIENTED_EDGE ( 'NONE', *, *, #11604, .F. ) ;
#20432 = CARTESIAN_POINT ( 'NONE',  ( 43.01140435219951286, 109.1297705074273239, 38.86567161673127657 ) ) ;
#20433 = DIRECTION ( 'NONE',  ( 0.000000000000000000, 1.000000000000000000, 0.000000000000000000 ) ) ;
#20434 = CARTESIAN_POINT ( 'NONE',  ( 38.96631938032478359, 128.4844580088725934, 31.27175355779120025 ) ) ;
#20435 = CARTESIAN_POINT ( 'NONE',  ( 38.58424406990784661, 144.2651871740940237, 35.64915139335016647 ) ) ;
#20436 = CARTESIAN_POINT ( 'NONE',  ( 37.24990543953586553, 153.6521207556136517, 3.648881909465930828 ) ) ;
#20437 = CLOSED_SHELL ( 'NONE', ( #241, #2998, #763, #5953, #18936, #21306, #10722, #13266, #1642, #2047, #15664, #12010, #2875, #13677, #2275, #20699, #12854, #1335, #10348, #20039, #11134, #19305, #8257, #18103 ) ) ;
#20438 = LINE ( 'NONE', #8322, #2901 ) ;
#20439 = PLANE ( 'NONE',  #6048 ) ;
#20440 = CARTESIAN_POINT ( 'NONE',  ( -145.2889157411863721, -168.5391397928654840, 41.15050349809590102 ) ) ;
#20441 = CARTESIAN_POINT ( 'NONE',  ( 46.10157429594899270, 100.7604996726487485, 38.46393386101375711 ) ) ;
#20442 = CARTESIAN_POINT ( 'NONE',  ( 175.9120630731088397, 202.0864028065961122, 21.73429951086134082 ) ) ;
#20443 = CARTESIAN_POINT ( 'NONE',  ( 48.01140435219951996, 92.36049967264872862, 32.58608133808903773 ) ) ;
#20444 = CARTESIAN_POINT ( 'NONE',  ( 42.21948215057684450, 98.11133943119283174, 29.21067981925356705 ) ) ;
#20445 = CARTESIAN_POINT ( 'NONE',  ( 39.42975644700377558, 96.67977050742732104, 36.81289934271958941 ) ) ;
#20446 = CARTESIAN_POINT ( 'NONE',  ( 22.17150742865759483, 138.9041494244890771, -4.010207742755246052 ) ) ;
#20447 = CARTESIAN_POINT ( 'NONE',  ( -142.0420953463935803, -177.2438272943107620, 46.59394152635518793 ) ) ;
#20448 = CARTESIAN_POINT ( 'NONE',  ( 44.37947211624943833, 83.21518717409399812, 30.00020018409699318 ) ) ;
#20449 = CYLINDRICAL_SURFACE ( 'NONE', #3245, 4.999999999999997335 ) ;
#20450 = CARTESIAN_POINT ( 'NONE',  ( -161.4692556286852891, -158.3391397928654385, 52.90620854394536821 ) ) ;
#20451 = ORIENTED_EDGE ( 'NONE', *, *, #1506, .F. ) ;
#20452 = CARTESIAN_POINT ( 'NONE',  ( 41.46631938032478359, 138.3844580088725991, 38.96596240072933170 ) ) ;
#20453 = FACE_OUTER_BOUND ( 'NONE', #20860, .T. ) ;
#20454 = CARTESIAN_POINT ( 'NONE',  ( 38.58424406990786082, 141.3797705074273381, 34.21067981925357060 ) ) ;
#20455 = CARTESIAN_POINT ( 'NONE',  ( 25.52315018325464635, 97.88680518890443238, 9.160641959101482712 ) ) ;
#20456 = ORIENTED_EDGE ( 'NONE', *, *, #20038, .T. ) ;
#20457 = EDGE_CURVE ( 'NONE', #11797, #9338, #8446, .T. ) ;
#20458 = DIRECTION ( 'NONE',  ( 0.5061580162706794672, 0.8624407588727068807, 0.000000000000000000 ) ) ;
#20459 = ORIENTED_EDGE ( 'NONE', *, *, #2304, .F. ) ;
#20460 = CARTESIAN_POINT ( 'NONE',  ( 46.59305225739526435, 134.1797705074273210, 31.60846029578754468 ) ) ;
#20461 = CARTESIAN_POINT ( 'NONE',  ( 137.5268905834513191, 193.0332408774651185, -19.99999999999997868 ) ) ;
#20462 = CARTESIAN_POINT ( 'NONE',  ( 46.59305225739526435, 61.91518717409400097, 31.60846029578754468 ) ) ;
#20463 = DIRECTION ( 'NONE',  ( -0.000000000000000000, -0.000000000000000000, 1.000000000000000000 ) ) ;
#20464 = CARTESIAN_POINT ( 'NONE',  ( 43.01140435219951996, 10.71049967264875491, 39.21067981925356349 ) ) ;
#20465 = CARTESIAN_POINT ( 'NONE',  ( 40.27526882409969033, 95.66518717409398675, 30.44471234641811819 ) ) ;
#20466 = CARTESIAN_POINT ( 'NONE',  ( -151.4692556286852891, -155.6438272943107393, 39.74470866294723947 ) ) ;
#20467 = CARTESIAN_POINT ( 'NONE',  ( 24.43941541943582862, 313.3049502139530205, 272.0939500981630204 ) ) ;
#20468 = CARTESIAN_POINT ( 'NONE',  ( -151.4692556286852891, -170.3130981290892692, 39.14238933923362396 ) ) ;
#20469 = DIRECTION ( 'NONE',  ( 0.6000000000000013101, -5.551115123125782702E-17, 0.7999999999999990452 ) ) ;
#20470 = CARTESIAN_POINT ( 'NONE',  ( -154.5594255724347761, -190.8891397928654783, 59.16757674456785310 ) ) ;
#20471 = CARTESIAN_POINT ( 'NONE',  ( 39.92123440845004723, 138.2344580088725650, 38.46393386101376421 ) ) ;
#20472 = CARTESIAN_POINT ( 'NONE',  ( 44.37947211624943833, 124.2797705074273154, 38.42115945441014446 ) ) ;
#20473 = CARTESIAN_POINT ( 'NONE',  ( 21.96620680132455306, 138.7984961796735490, 1.985398331534963923 ) ) ;
#20474 = DIRECTION ( 'NONE',  ( -0.000000000000000000, -0.000000000000000000, -1.000000000000000000 ) ) ;
#20475 = CARTESIAN_POINT ( 'NONE',  ( 47.43856463449117911, 109.4651871740940123, 35.64915139335015937 ) ) ;
#20476 = CARTESIAN_POINT ( 'NONE',  ( -151.4692556286853176, -180.2391397928654726, 39.65701158161629536 ) ) ;
#20477 = CARTESIAN_POINT ( 'NONE',  ( 63.55746018358933469, 147.2895578332197033, -9.446739241148069510 ) ) ;
#20478 =( BOUNDED_CURVE ( )  B_SPLINE_CURVE ( 2, ( #21785, #11958, #16695, #20133, #11627, #11736, #18357, #18689, #6692, #17128, #6903, #3696, #18793 ),
 .UNSPECIFIED., .F., .T. ) 
 B_SPLINE_CURVE_WITH_KNOTS ( ( 3, 2, 2, 2, 2, 2, 3 ),
 ( 0.1249999999999999584, 0.1285714285714285587, 0.1357142857142857040, 0.1428571428571428492, 0.1499999999999999944, 0.1571428571428571397, 0.1607142857142856707 ),
 .UNSPECIFIED. ) 
 CURVE ( )  GEOMETRIC_REPRESENTATION_ITEM ( )  RATIONAL_B_SPLINE_CURVE ( ( 0.9755282581475768211, 0.9755282581475765991, 1.000000000000000000, 0.9510565162951535312, 1.000000000000000000, 0.9510565162951535312, 1.000000000000000000, 0.9510565162951535312, 1.000000000000000000, 0.9510565162951535312, 1.000000000000000000, 0.9755282581475770431, 0.9755282581475765991 ) ) 
 REPRESENTATION_ITEM ( '' )  );
#20479 = CARTESIAN_POINT ( 'NONE',  ( 70.51576897149806200, 126.1317638695992116, 12.41827883020830470 ) ) ;
#20480 = ADVANCED_FACE ( 'NONE', ( #16728 ), #12092, .T. ) ;
#20481 = CARTESIAN_POINT ( 'NONE',  ( -151.4692556286852607, -156.8130981290892692, 59.65701158161632378 ) ) ;
#20482 = AXIS2_PLACEMENT_3D ( 'NONE', #363, #3887, #12252 ) ;
#20483 = CARTESIAN_POINT ( 'NONE',  ( 45.74753988029934249, 86.32977050742731251, 30.44471234641812174 ) ) ;
#20484 = EDGE_LOOP ( 'NONE', ( #8256, #10531, #21132, #21404 ) ) ;
#20485 = CARTESIAN_POINT ( 'NONE',  ( 48.01140435219951996, 139.4344580088725536, 32.58608133808903773 ) ) ;
#20486 = CARTESIAN_POINT ( 'NONE',  ( 38.01140435219951996, 77.63445800887255643, 32.58608133808903773 ) ) ;
#20487 = CARTESIAN_POINT ( 'NONE',  ( 38.96631938032478359, 59.48445800887257207, 31.27175355779120025 ) ) ;
#20488 = CARTESIAN_POINT ( 'NONE',  ( 46.10157429594899270, 131.6604996726487116, 29.95742577749337343 ) ) ;
#20490 = CARTESIAN_POINT ( 'NONE',  ( 21.13084688720937976, 146.0403058103794649, -16.94226050084479596 ) ) ;
#20489 = CARTESIAN_POINT ( 'NONE',  ( 44.37947211624943833, 92.21518717409401233, 30.00020018409699318 ) ) ;
#20491 = B_SPLINE_CURVE_WITH_KNOTS ( 'NONE', 3,
 ( #4425, #9628, #7971, #21418, #6307, #19758, #13472, #20204, #5312, #16983, #4990, #10390, #3335, #8735, #11700, #3554, #19989, #21642, #6977, #8627, #18435, #10063, #12023, #20101, #5097, #1792, #6656, #11814, #8523, #4875, #21747, #6865, #1891, #15345, #17090, #15237 ),
 .UNSPECIFIED., .F., .F.,
 ( 4, 2, 2, 2, 2, 2, 2, 2, 2, 2, 2, 2, 2, 2, 2, 2, 2, 4 ),
 ( 6.938893903907227607E-18, 0.0009794911224654358813, 0.001958982244930864824, 0.002938473367396293983, 0.003917964489861722709, 0.004897455612327151868, 0.005876946734792581027, 0.006856437857258010186, 0.007835928979723438478, 0.008815420102188867638, 0.009794911224654296797, 0.01028465678588701658, 0.01077440234711973810, 0.01175389346958516552, 0.01273338459205059121, 0.01371287571451601690, 0.01469236683698144086, 0.01567185795944686655 ),
 .UNSPECIFIED. ) ;
#20492 = CARTESIAN_POINT ( 'NONE',  ( -154.3824083646099439, -160.5584106276440366, 58.62277379824867296 ) ) ;
#20493 = CARTESIAN_POINT ( 'NONE',  ( -154.3824083646099439, -179.4938272943107336, 40.69124936498395328 ) ) ;
#20494 = CARTESIAN_POINT ( 'NONE',  ( -148.3790856849358306, -177.3891397928654783, 40.14644641866477315 ) ) ;
#20495 = DIRECTION ( 'NONE',  ( 0.7066505893342458489, 0.7066505893340067068, 0.03591502732094190020 ) ) ;
#20496 = AXIS2_PLACEMENT_3D ( 'NONE', #11503, #8435, #11945 ) ;
#20497 = CARTESIAN_POINT ( 'NONE',  ( 39.92123440845005433, 92.33445800887255928, 29.95742577749336988 ) ) ;
#20498 = CARTESIAN_POINT ( 'NONE',  ( -161.4692556286852891, -173.3391397928654385, 52.90620854394536821 ) ) ;
#20499 = CARTESIAN_POINT ( 'NONE',  ( 39.42975644700377558, 153.0797705074273267, 31.60846029578754468 ) ) ;
#20500 = CARTESIAN_POINT ( 'NONE',  ( 39.42975644700377558, 102.6797705074273210, 36.81289934271958941 ) ) ;
#20501 = CARTESIAN_POINT ( 'NONE',  ( 63.43270131736515083, 147.4839633491013728, -3.451138109367889228 ) ) ;
#20502 = CARTESIAN_POINT ( 'NONE',  ( 47.43856463449117911, 139.7651871740939953, 32.77220824515697473 ) ) ;
#20503 = AXIS2_PLACEMENT_3D ( 'NONE', #18379, #10010, #19400 ) ;
#20504 = CARTESIAN_POINT ( 'NONE',  ( 43.01140435219951286, 66.53445800887257633, 39.21067981925356349 ) ) ;
#20505 = CARTESIAN_POINT ( 'NONE',  ( -145.6429501568359797, -162.2084106276440423, 41.63779006702063867 ) ) ;
#20506 = CARTESIAN_POINT ( 'NONE',  ( 43.01140435219951996, 119.9070776186055838, 50.00000000000002842 ) ) ;
#20507 = CARTESIAN_POINT ( 'NONE',  ( 17.92634965299622252, 143.2997274935095788, 22.91961472066619265 ) ) ;
#20508 = LINE ( 'NONE', #17180, #14789 ) ;
#20509 = CARTESIAN_POINT ( 'NONE',  ( 40.27526882409969033, 113.6651871740939868, 30.44471234641811819 ) ) ;
#20510 = VERTEX_POINT ( 'NONE', #5162 ) ;
#20511 = CARTESIAN_POINT ( 'NONE',  ( -157.6495955161842062, -179.9391397928654328, 41.15050349809589392 ) ) ;
#20512 = EDGE_CURVE ( 'NONE', #2203, #17644, #9131, .T. ) ;
#20513 = ORIENTED_EDGE ( 'NONE', *, *, #6806, .T. ) ;
#20514 = CARTESIAN_POINT ( 'NONE',  ( 48.01140435219951996, 97.13445800887258486, 35.83527830041810347 ) ) ;
#20515 = CARTESIAN_POINT ( 'NONE',  ( 38.58424406990784661, 60.22977050742731109, 32.77220824515698183 ) ) ;
#20517 = CARTESIAN_POINT ( 'NONE',  ( 49.88381083390898851, 92.64041853056629350, -12.86295667411130239 ) ) ;
#20516 = CARTESIAN_POINT ( 'NONE',  ( 45.74753988029933538, 116.0651871740939924, 30.44471234641811819 ) ) ;
#20518 = CARTESIAN_POINT ( 'NONE',  ( 47.05648932407426344, 73.91049967264873999, 37.14960608071593384 ) ) ;
#20520 = DIRECTION ( 'NONE',  ( 0.000000000000000000, -1.000000000000000000, 0.000000000000000000 ) ) ;
#20519 = DIRECTION ( 'NONE',  ( -0.000000000000000000, -0.000000000000000000, -1.000000000000000000 ) ) ;
#20521 = CARTESIAN_POINT ( 'NONE',  ( 42.21948215057687293, 71.11133943119284595, 29.21067981925355994 ) ) ;
#20522 = CARTESIAN_POINT ( 'NONE',  ( 45.23168579428472924, 95.00401654713870414, 38.70263932541809737 ) ) ;
#20523 = CARTESIAN_POINT ( 'NONE',  ( 38.58424406990784661, 78.26518717409400949, 35.64915139335016647 ) ) ;
#20524 = DIRECTION ( 'NONE',  ( -0.9393725726208707050, -0.3428981916074316794, -0.000000000000000000 ) ) ;
#20525 = CARTESIAN_POINT ( 'NONE',  ( -145.6429501568359797, -182.9438272943106938, 41.63779006702063867 ) ) ;
#20526 = FACE_OUTER_BOUND ( 'NONE', #6780, .T. ) ;
#20527 = EDGE_CURVE ( 'NONE', #19772, #17982, #10133, .T. ) ;
#20528 = ORIENTED_EDGE ( 'NONE', *, *, #17428, .F. ) ;
#20529 = CARTESIAN_POINT ( 'NONE',  ( -142.0420953463935803, -189.8084106276440366, 52.72008163687743831 ) ) ;
#20530 = CARTESIAN_POINT ( 'NONE',  ( 21.90415124324598750, 92.95514585177724598, 15.07745334355238676 ) ) ;
#20531 = ORIENTED_EDGE ( 'NONE', *, *, #14159, .F. ) ;
#20532 = CARTESIAN_POINT ( 'NONE',  ( 46.59305225739526435, 139.3151871740940067, 36.81289934271958941 ) ) ;
#20533 = CARTESIAN_POINT ( 'NONE',  ( 45.74753988029934249, 158.0651871740940067, 30.44471234641812174 ) ) ;
#20534 = ADVANCED_FACE ( 'NONE', ( #5273 ), #20062, .T. ) ;
#20535 = CARTESIAN_POINT ( 'NONE',  ( 39.42975644700377558, 105.6797705074273352, 36.81289934271958941 ) ) ;
#20536 = CARTESIAN_POINT ( 'NONE',  ( 14.88286428391304561, 100.3963227437532595, 8.410691821786379307 ) ) ;
#20537 = ORIENTED_EDGE ( 'NONE', *, *, #18540, .T. ) ;
#20538 = CARTESIAN_POINT ( 'NONE',  ( 51.84853669763433004, 93.12814091139611605, 7.061107544354192633 ) ) ;
#20539 = ORIENTED_EDGE ( 'NONE', *, *, #20679, .F. ) ;
#20540 = CARTESIAN_POINT ( 'NONE',  ( 40.27526882409969033, 108.8297705074272983, 37.97664729208901946 ) ) ;
#20541 = EDGE_CURVE ( 'NONE', #5132, #17319, #8485, .T. ) ;
#20542 = FACE_OUTER_BOUND ( 'NONE', #2349, .T. ) ;
#20543 = CARTESIAN_POINT ( 'NONE',  ( -151.4692556286852891, -196.9891397928655010, 39.65701158161630246 ) ) ;
#20544 = CARTESIAN_POINT ( 'NONE',  ( 44.37947211624943833, 82.27977050742732956, 38.42115945441014446 ) ) ;
#20545 = CARTESIAN_POINT ( 'NONE',  ( 40.27526882409969033, 140.6651871740939725, 30.44471234641811819 ) ) ;
#20546 = CARTESIAN_POINT ( 'NONE',  ( 38.01140435219952707, 105.7104996726487371, 34.21067981925357060 ) ) ;
#20547 = CARTESIAN_POINT ( 'NONE',  ( 44.41273964558330789, 85.70220254879866673, -6.708519844216274564 ) ) ;
#20548 = CARTESIAN_POINT ( 'NONE',  ( -145.2889157411863437, -179.6130981290892521, 41.15050349809589392 ) ) ;
#20549 = CARTESIAN_POINT ( 'NONE',  ( -141.4692556286852891, -168.8391397928654385, 46.40781461928724383 ) ) ;
#20550 = DIRECTION ( 'NONE',  ( 0.000000000000000000, 0.000000000000000000, 1.000000000000000000 ) ) ;
#20551 = UNCERTAINTY_MEASURE_WITH_UNIT (LENGTH_MEASURE( 1.000000000000000082E-05 ), #19886, 'distance_accuracy_value', 'NONE');
#20552 = DIRECTION ( 'NONE',  ( 0.000000000000000000, 0.000000000000000000, 1.000000000000000000 ) ) ;
#20553 = CARTESIAN_POINT ( 'NONE',  ( 47.05648932407426344, 76.91049967264873999, 37.14960608071593384 ) ) ;
#20554 = DIRECTION ( 'NONE',  ( -0.000000000000000000, -1.000000000000000000, -0.000000000000000000 ) ) ;
#20555 = CARTESIAN_POINT ( 'NONE',  ( 40.27526882409969033, 81.82977050742729830, 37.97664729208901946 ) ) ;
#20556 = CARTESIAN_POINT ( 'NONE',  ( 37.67147452025017174, 147.5968219552084122, -3.296006884014541782 ) ) ;
#20557 = CARTESIAN_POINT ( 'NONE',  ( -160.8964159109769696, -175.8938272943107393, 49.65701158161630957 ) ) ;
#20558 = CARTESIAN_POINT ( 'NONE',  ( 47.43856463449117911, 79.46518717409399812, 35.64915139335015937 ) ) ;
#20559 = CYLINDRICAL_SURFACE ( 'NONE', #12033, 10.00000000000000888 ) ;
#20560 = DIRECTION ( 'NONE',  ( -0.000000000000000000, -0.000000000000000000, -1.000000000000000000 ) ) ;
#20561 = EDGE_LOOP ( 'NONE', ( #8853, #18025 ) ) ;
#20562 = CARTESIAN_POINT ( 'NONE',  ( 38.01140435219952707, 117.8604996726487428, 35.83527830041809636 ) ) ;
#20563 = EDGE_CURVE ( 'NONE', #21618, #8176, #13354, .T. ) ;
#20564 = DIRECTION ( 'NONE',  ( -1.000000000000000000, 0.000000000000000000, 0.000000000000000000 ) ) ;
#20565 = CARTESIAN_POINT ( 'NONE',  ( 43.01140435219951286, 133.1297705074273381, 38.86567161673127657 ) ) ;
#20566 = CARTESIAN_POINT ( 'NONE',  ( 20.91795382191701336, 137.2581800298614212, 10.90446256675174297 ) ) ;
#20567 = ORIENTED_EDGE ( 'NONE', *, *, #12477, .F. ) ;
#20568 = EDGE_LOOP ( 'NONE', ( #9823, #15361, #14686, #16438 ) ) ;
#20569 = CARTESIAN_POINT ( 'NONE',  ( 38.58424406990786082, 132.3797705074273381, 34.21067981925357060 ) ) ;
#20570 = LINE ( 'NONE', #1729, #10451 ) ;
#20571 = VECTOR ( 'NONE', #6134, 1000.000000000000000 ) ;
#20572 = CARTESIAN_POINT ( 'NONE',  ( 39.42975644700377558, 96.41518717409400097, 36.81289934271958941 ) ) ;
#20573 = CARTESIAN_POINT ( 'NONE',  ( -145.6429501568359797, -156.8438272943107279, 57.67623309621197336 ) ) ;
#20574 = DIRECTION ( 'NONE',  ( 0.000000000000000000, 0.000000000000000000, -1.000000000000000000 ) ) ;
#20575 = CARTESIAN_POINT ( 'NONE',  ( -143.3790856849358306, -170.7630981290892862, 43.77915905869157598 ) ) ;
#20576 = EDGE_CURVE ( 'NONE', #19216, #8279, #6725, .T. ) ;
#20577 = CARTESIAN_POINT ( 'NONE',  ( 39.92123440845004723, 146.3344580088725593, 29.95742577749337343 ) ) ;
#20578 = CARTESIAN_POINT ( 'NONE',  ( 47.43856463449117200, 109.7297705074273040, 35.64915139335016647 ) ) ;
#20579 = CARTESIAN_POINT ( 'NONE',  ( 57.25245068215419053, 144.3413351293631877, -3.490753295080526453 ) ) ;
#20580 = CARTESIAN_POINT ( 'NONE',  ( -145.2889157411863437, -184.4391397928654328, 58.16351966513671812 ) ) ;
#20581 = CARTESIAN_POINT ( 'NONE',  ( 39.42975644700377558, 102.4151871740940010, 36.81289934271958941 ) ) ;
#20582 = ORIENTED_EDGE ( 'NONE', *, *, #1254, .F. ) ;
#20583 = CYLINDRICAL_SURFACE ( 'NONE', #975, 576.1986910693910886 ) ;
#20584 = CARTESIAN_POINT ( 'NONE',  ( 9.345857484954766647, 125.6588058825717837, 10.27205150250232535 ) ) ;
#20585 = CARTESIAN_POINT ( 'NONE',  ( 69.85845278386915425, 111.2786852186620621, 13.01367670771671747 ) ) ;
#20586 = ADVANCED_BREP_SHAPE_REPRESENTATION ( '', ( #7102, #12657 ), #4220 ) ;
#20587 = CARTESIAN_POINT ( 'NONE',  ( 149.5529451524149920, 187.4828467975320336, 34.00000000000001421 ) ) ;
#20588 = CARTESIAN_POINT ( 'NONE',  ( 40.27526882409969744, 89.92977050742732104, 30.44471234641812174 ) ) ;
#20589 = VECTOR ( 'NONE', #14293, 1000.000000000000000 ) ;
#20590 = ORIENTED_EDGE ( 'NONE', *, *, #11064, .T. ) ;
#20591 = CARTESIAN_POINT ( 'NONE',  ( 48.01140435219951996, 73.13445800887258486, 35.83527830041810347 ) ) ;
#20592 = CARTESIAN_POINT ( 'NONE',  ( -143.3790856849358306, -164.7630981290893146, 43.77915905869157598 ) ) ;
#20593 = CARTESIAN_POINT ( 'NONE',  ( 44.55648932407425633, 127.6104996726487570, 38.96596240072933170 ) ) ;
#20595 = CARTESIAN_POINT ( 'NONE',  ( 29.11053999216420252, 151.1052802516552163, -16.63225393015772724 ) ) ;
#20594 = CARTESIAN_POINT ( 'NONE',  ( 39.42975644700377558, 90.41518717409400097, 36.81289934271958941 ) ) ;
#20596 = CARTESIAN_POINT ( 'NONE',  ( -151.4692556286852891, -195.2391397928654726, 39.14238933923362396 ) ) ;
#20597 = EDGE_CURVE ( 'NONE', #11299, #4102, #20170, .T. ) ;
#20598 = CARTESIAN_POINT ( 'NONE',  ( -157.2955611005345986, -182.3438272943106995, 41.63779006702063867 ) ) ;
#20599 = CARTESIAN_POINT ( 'NONE',  ( 43.01140435219951286, 86.96049967264872294, 29.21067981925356705 ) ) ;
#20600 = CARTESIAN_POINT ( 'NONE',  ( 47.05648932407426344, 127.5844580088725877, 31.27175355779120025 ) ) ;
#20601 = DIRECTION ( 'NONE',  ( 0.000000000000000000, 1.000000000000000000, 0.000000000000000000 ) ) ;
#20602 = CARTESIAN_POINT ( 'NONE',  ( 47.05648932407426344, 142.9104996726487400, 37.14960608071593384 ) ) ;
#20603 = CARTESIAN_POINT ( 'NONE',  ( 44.37947211624943833, 152.4797705074273324, 30.00020018409699318 ) ) ;
#20604 =( BOUNDED_CURVE ( )  B_SPLINE_CURVE ( 2, ( #725, #9323, #14162, #19239, #11070, #15709, #12621, #9437, #5998, #14263, #4139, #4242, #614 ),
 .UNSPECIFIED., .F., .T. ) 
 B_SPLINE_CURVE_WITH_KNOTS ( ( 3, 2, 2, 2, 2, 2, 3 ),
 ( 0.3308823529411764608, 0.3323529411764705732, 0.3352941176470587981, 0.3382352941176470784, 0.3411764705882353033, 0.3441176470588235281, 0.3455882352941176405 ),
 .UNSPECIFIED. ) 
 CURVE ( )  GEOMETRIC_REPRESENTATION_ITEM ( )  RATIONAL_B_SPLINE_CURVE ( ( 0.9755282581475768211, 0.9755282581475768211, 1.000000000000000000, 0.9510565162951535312, 1.000000000000000000, 0.9510565162951535312, 1.000000000000000000, 0.9510565162951535312, 1.000000000000000000, 0.9510565162951535312, 1.000000000000000000, 0.9755282581475768211, 0.9755282581475768211 ) ) 
 REPRESENTATION_ITEM ( '' )  );
#20605 = CARTESIAN_POINT ( 'NONE',  ( 40.27526882409969033, 104.9297705074273210, 30.44471234641811819 ) ) ;
#20606 = CARTESIAN_POINT ( 'NONE',  ( 75.87089013534350102, 129.7906142932847331, -2.736556584054479657 ) ) ;
#20607 = CARTESIAN_POINT ( 'NONE',  ( 47.43856463449117911, 136.4651871740939839, 35.64915139335015937 ) ) ;
#20608 = CARTESIAN_POINT ( 'NONE',  ( 48.01140435219951996, 67.28445800887257633, 34.21067981925357060 ) ) ;
#20609 = CARTESIAN_POINT ( 'NONE',  ( -142.0420953463936087, -168.6584106276440593, 49.65701158161630957 ) ) ;
#20610 = CARTESIAN_POINT ( 'NONE',  ( 43.01140435219951286, 117.5344580088725763, 39.21067981925356349 ) ) ;
#20611 = ADVANCED_FACE ( 'NONE', ( #98 ), #16941, .F. ) ;
#20612 = CARTESIAN_POINT ( 'NONE',  ( 46.79023103138236905, 91.88018867020078062, 6.271112617211819007 ) ) ;
#20613 = DIRECTION ( 'NONE',  ( -0.000000000000000000, 1.000000000000000000, -0.000000000000000000 ) ) ;
#20614 = CARTESIAN_POINT ( 'NONE',  ( 38.58424406990784661, 116.9651871740939839, 32.77220824515698183 ) ) ;
#20615 = VERTEX_POINT ( 'NONE', #15616 ) ;
#20616 = EDGE_CURVE ( 'NONE', #13985, #9753, #14286, .T. ) ;
#20617 = CARTESIAN_POINT ( 'NONE',  ( 43.01140435219951286, 114.5344580088725621, 39.21067981925356349 ) ) ;
#20618 = ORIENTED_EDGE ( 'NONE', *, *, #3330, .T. ) ;
#20619 = CARTESIAN_POINT ( 'NONE',  ( 44.55648932407425633, 99.68445800887256780, 38.96596240072933170 ) ) ;
#20620 = CARTESIAN_POINT ( 'NONE',  ( 44.37947211624943833, 148.2797705074273154, 38.42115945441014446 ) ) ;
#20621 = CARTESIAN_POINT ( 'NONE',  ( 38.01140435219951996, 153.8604996726487002, 35.83527830041810347 ) ) ;
#20623 = CARTESIAN_POINT ( 'NONE',  ( 71.20918238807936973, 120.1790618917378879, 12.65642078274776416 ) ) ;
#20622 = CARTESIAN_POINT ( 'NONE',  ( 38.58424406990786082, 117.1151871740940038, 34.21067981925357060 ) ) ;
#20624 = CARTESIAN_POINT ( 'NONE',  ( 47.05648932407426344, 67.91049967264873999, 37.14960608071593384 ) ) ;
#20626 = FACE_OUTER_BOUND ( 'NONE', #19745, .T. ) ;
#20625 = CARTESIAN_POINT ( 'NONE',  ( -141.4692556286852891, -195.0630981290893260, 49.65701158161630957 ) ) ;
#20627 = AXIS2_PLACEMENT_3D ( 'NONE', #20955, #9381, #886 ) ;
#20628 = DIRECTION ( 'NONE',  ( 0.000000000000000000, 0.000000000000000000, 1.000000000000000000 ) ) ;
#20629 = CARTESIAN_POINT ( 'NONE',  ( 46.31425486152256354, 95.12510261592046845, 30.44250125826514974 ) ) ;
#20630 = CARTESIAN_POINT ( 'NONE',  ( 40.27526882409969033, 80.66518717409400097, 30.44471234641811819 ) ) ;
#20631 = CARTESIAN_POINT ( 'NONE',  ( 44.55648932407425633, 104.8104996726487457, 29.45539723777780239 ) ) ;
#20632 = CARTESIAN_POINT ( 'NONE',  ( -142.0420953463935803, -183.5438272943107449, 52.72008163687743831 ) ) ;
#20633 = CARTESIAN_POINT ( 'NONE',  ( -160.8964159109769696, -191.3084106276440650, 46.59394152635518083 ) ) ;
#20634 = EDGE_LOOP ( 'NONE', ( #11608, #9230 ) ) ;
#20635 = EDGE_CURVE ( 'NONE', #7574, #13720, #15324, .T. ) ;
#20636 = CARTESIAN_POINT ( 'NONE',  ( -151.4692556286852891, -176.9084106276440309, 39.74470866294723947 ) ) ;
#20637 = CARTESIAN_POINT ( 'NONE',  ( 40.68735894681399401, 154.1427111589966898, 9.763412716672732472 ) ) ;
#20638 = ORIENTED_EDGE ( 'NONE', *, *, #15368, .T. ) ;
#20639 = CARTESIAN_POINT ( 'NONE',  ( 43.01140435219951286, 147.8651871740940180, 38.86567161673127657 ) ) ;
#20640 = DIRECTION ( 'NONE',  ( 0.8654262854811264338, 0.000000000000000000, -0.5010362705417042983 ) ) ;
#20641 = CARTESIAN_POINT ( 'NONE',  ( 46.59305225739526435, 104.1797705074273210, 31.60846029578754468 ) ) ;
#20642 = CARTESIAN_POINT ( 'NONE',  ( 20.22230697948889500, 94.36241449208007737, 1.148710122009321211 ) ) ;
#20643 = ORIENTED_EDGE ( 'NONE', *, *, #6973, .T. ) ;
#20644 = CARTESIAN_POINT ( 'NONE',  ( 15.96294818963569639, 111.9339314265907745, 8.846935114401974332 ) ) ;
#20645 = AXIS2_PLACEMENT_3D ( 'NONE', #5271, #13639, #14255 ) ;
#20646 = ORIENTED_EDGE ( 'NONE', *, *, #19160, .F. ) ;
#20647 = DIRECTION ( 'NONE',  ( 0.2767211344570353337, -0.9609502660100633920, 0.000000000000000000 ) ) ;
#20648 = DIRECTION ( 'NONE',  ( -0.000000000000000000, -0.000000000000000000, -1.000000000000000000 ) ) ;
#20649 = CARTESIAN_POINT ( 'NONE',  ( 44.37947211624943833, 142.0151871740939953, 38.42115945441014446 ) ) ;
#20650 = EDGE_CURVE ( 'NONE', #8279, #6960, #15832, .T. ) ;
#20651 = CARTESIAN_POINT ( 'NONE',  ( 48.01140435219951996, 101.3604996726487286, 32.58608133808903773 ) ) ;
#20652 = CARTESIAN_POINT ( 'NONE',  ( 15.75986397150585816, 99.18880659646561071, -5.637120474378671808 ) ) ;
#20653 = CARTESIAN_POINT ( 'NONE',  ( 136.2512292229016566, 181.9026294830433699, 20.77285216529425682 ) ) ;
#20654 = CARTESIAN_POINT ( 'NONE',  ( -141.4692556286852891, -171.9891397928654726, 49.65701158161630957 ) ) ;
#20655 = EDGE_CURVE ( 'NONE', #5468, #12794, #2499, .T. ) ;
#20656 = CIRCLE ( 'NONE', #6579, 7.500000000000007105 ) ;
#20657 = LINE ( 'NONE', #3475, #14347 ) ;
#20658 = CARTESIAN_POINT ( 'NONE',  ( -151.4692556286852891, -195.9891397928654726, 39.65701158161630246 ) ) ;
#20659 = LINE ( 'NONE', #12268, #4285 ) ;
#20660 = VECTOR ( 'NONE', #9535, 1000.000000000000000 ) ;
#20661 = CARTESIAN_POINT ( 'NONE',  ( 47.43856463449117200, 86.02977050742731535, 32.77220824515698183 ) ) ;
#20662 = CARTESIAN_POINT ( 'NONE',  ( -157.2955611005346270, -166.4438272943107506, 57.67623309621198047 ) ) ;
#20663 = CARTESIAN_POINT ( 'NONE',  ( 38.58424406990785371, 80.96518717409399812, 32.77220824515697473 ) ) ;
#20664 = DIRECTION ( 'NONE',  ( -1.000000000000000000, 0.000000000000000000, -0.000000000000000000 ) ) ;
#20665 = DIRECTION ( 'NONE',  ( 0.000000000000000000, 0.000000000000000000, 1.000000000000000000 ) ) ;
#20666 = EDGE_LOOP ( 'NONE', ( #7064, #12994, #13877, #10019 ) ) ;
#20667 = DIRECTION ( 'NONE',  ( 0.000000000000000000, 1.000000000000000000, 0.000000000000000000 ) ) ;
#20668 =( BOUNDED_CURVE ( )  B_SPLINE_CURVE ( 2, ( #18669, #3572, #15470, #7099, #8643, #2126, #6994 ),
 .UNSPECIFIED., .F., .F. ) 
 B_SPLINE_CURVE_WITH_KNOTS ( ( 3, 2, 2, 3 ),
 ( 0.000000000000000000, 0.002941176470588235253, 0.005882352941176470507, 0.007352941176470595072 ),
 .UNSPECIFIED. ) 
 CURVE ( )  GEOMETRIC_REPRESENTATION_ITEM ( )  RATIONAL_B_SPLINE_CURVE ( ( 1.000000000000000000, 0.9510565162951535312, 1.000000000000000000, 0.9510565162951535312, 1.000000000000000000, 0.9755282581475765991, 0.9755282581475767101 ) ) 
 REPRESENTATION_ITEM ( '' )  );
#20669 = CARTESIAN_POINT ( 'NONE',  ( 46.59305225739526435, 134.1797705074273210, 31.60846029578754468 ) ) ;
#20670 = CARTESIAN_POINT ( 'NONE',  ( 71.13077487245369923, 119.9619191372588034, 6.660813687590150245 ) ) ;
#20671 = ORIENTED_EDGE ( 'NONE', *, *, #12070, .T. ) ;
#20672 = CARTESIAN_POINT ( 'NONE',  ( 48.01140435219951996, 73.28445800887257633, 34.21067981925357060 ) ) ;
#20673 = ORIENTED_EDGE ( 'NONE', *, *, #15163, .T. ) ;
#20674 = AXIS2_PLACEMENT_3D ( 'NONE', #2213, #20121, #7403 ) ;
#20675 = CARTESIAN_POINT ( 'NONE',  ( 41.64333658814960870, 138.9797705074273324, 38.42115945441014446 ) ) ;
#20676 = CARTESIAN_POINT ( 'NONE',  ( 43.01140435219951286, 91.12977050742732388, 38.86567161673127657 ) ) ;
#20677 = FACE_OUTER_BOUND ( 'NONE', #20090, .T. ) ;
#20678 = CARTESIAN_POINT ( 'NONE',  ( 44.55648932407425633, 121.8844580088725849, 29.45539723777780239 ) ) ;
#20679 = EDGE_CURVE ( 'NONE', #11465, #9722, #15111, .T. ) ;
#20680 = CARTESIAN_POINT ( 'NONE',  ( 39.42975644700377558, 95.81518717409399244, 31.60846029578754468 ) ) ;
#20681 = DIRECTION ( 'NONE',  ( 1.000000000000000000, 0.000000000000000000, 0.000000000000000000 ) ) ;
#20682 = LINE ( 'NONE', #5567, #13910 ) ;
#20683 = CARTESIAN_POINT ( 'NONE',  ( -159.5594255724347761, -163.8630981290893089, 43.77915905869157598 ) ) ;
#20684 = CARTESIAN_POINT ( 'NONE',  ( -157.6495955161842062, -191.0391397928654271, 58.16351966513671812 ) ) ;
#20685 = CARTESIAN_POINT ( 'NONE',  ( 46.10157429594899270, 142.7344580088725934, 29.95742577749337343 ) ) ;
#20686 = CARTESIAN_POINT ( 'NONE',  ( 38.58424406990784661, 114.2297705074273040, 32.77220824515698183 ) ) ;
#20687 = CARTESIAN_POINT ( 'NONE',  ( 22.89857099655110062, 139.5608133708311982, -4.966967973427480310 ) ) ;
#20688 = DIRECTION ( 'NONE',  ( 0.000000000000000000, -1.000000000000000000, -0.000000000000000000 ) ) ;
#20689 = CARTESIAN_POINT ( 'NONE',  ( 41.64333658814960870, 107.5151871740939953, 30.00020018409699318 ) ) ;
#20690 = CIRCLE ( 'NONE', #3789, 7.500000000000007105 ) ;
#20691 = ORIENTED_EDGE ( 'NONE', *, *, #18308, .T. ) ;
#20692 = CARTESIAN_POINT ( 'NONE',  ( 43.01140435219951996, 10.71049967264875491, 34.21067981925357060 ) ) ;
#20693 = CARTESIAN_POINT ( 'NONE',  ( 15.39564893635072806, 140.1373336744895255, -4.208549045858890558 ) ) ;
#20694 = CARTESIAN_POINT ( 'NONE',  ( 70.03002323795641360, 111.8333997399938511, 5.989792257250448060 ) ) ;
#20695 = PLANE ( 'NONE',  #7585 ) ;
#20696 = CARTESIAN_POINT ( 'NONE',  ( 38.58424406990786082, 78.37977050742732388, 34.21067981925357060 ) ) ;
#20697 = ORIENTED_EDGE ( 'NONE', *, *, #13920, .F. ) ;
#20698 = VECTOR ( 'NONE', #8033, 1000.000000000000000 ) ;
#20699 = ADVANCED_FACE ( 'NONE', ( #10890, #4160, #20809, #9241 ), #5700, .T. ) ;
#20700 = VECTOR ( 'NONE', #14062, 1000.000000000000114 ) ;
#20701 = CARTESIAN_POINT ( 'NONE',  ( 41.46631938032478359, 66.38445800887257064, 38.96596240072933170 ) ) ;
#20702 = CIRCLE ( 'NONE', #12194, 21.90454335994848734 ) ;
#20703 = CARTESIAN_POINT ( 'NONE',  ( 38.96631938032478359, 130.0104996726487343, 37.14960608071593384 ) ) ;
#20705 = CARTESIAN_POINT ( 'NONE',  ( 77.15557362092413030, 120.6950048976143250, -0.4420599252208967100 ) ) ;
#20704 = CARTESIAN_POINT ( 'NONE',  ( 38.58424406990786082, 90.11518717409400381, 34.21067981925357060 ) ) ;
#20706 = CARTESIAN_POINT ( 'NONE',  ( -142.0420953463936087, -183.3938272943107108, 49.65701158161630957 ) ) ;
#20707 = CARTESIAN_POINT ( 'NONE',  ( 38.96631938032478359, 116.4844580088725792, 31.27175355779120025 ) ) ;
#20708 = FACE_OUTER_BOUND ( 'NONE', #5006, .T. ) ;
#20709 = CARTESIAN_POINT ( 'NONE',  ( 39.92123440845005433, 81.23445800887256496, 38.46393386101375711 ) ) ;
#20710 = CARTESIAN_POINT ( 'NONE',  ( 48.01140435219951996, 143.3604996726487570, 32.58608133808903773 ) ) ;
#20711 = CARTESIAN_POINT ( 'NONE',  ( 47.43856463449118621, 142.8797705074273381, 34.21067981925357060 ) ) ;
#20712 = CARTESIAN_POINT ( 'NONE',  ( 38.58424406990784661, 108.2297705074273182, 32.77220824515698183 ) ) ;
#20713 = CARTESIAN_POINT ( 'NONE',  ( 10.91571581598819662, 131.8149664739095783, 9.482090752819161139 ) ) ;
#20714 = CARTESIAN_POINT ( 'NONE',  ( 41.64333658814960870, 137.5151871740939953, 30.00020018409699318 ) ) ;
#20715 = CARTESIAN_POINT ( 'NONE',  ( -143.8425227516148084, -156.0938272943107279, 44.11586579668791330 ) ) ;
#20716 = CARTESIAN_POINT ( 'NONE',  ( -160.8964159109769696, -167.1584106276440593, 49.65701158161630957 ) ) ;
#20717 = CARTESIAN_POINT ( 'NONE',  ( -157.6495955161842062, -164.9391397928654612, 41.15050349809589392 ) ) ;
#20718 = CARTESIAN_POINT ( 'NONE',  ( 48.01140435219951996, 91.13445800887257064, 35.83527830041809636 ) ) ;
#20719 = CARTESIAN_POINT ( 'NONE',  ( 28.77282558494574971, 95.47244942437217219, 14.00900696324737282 ) ) ;
#20720 = DIRECTION ( 'NONE',  ( 0.000000000000000000, 0.000000000000000000, 1.000000000000000000 ) ) ;
#20721 = CARTESIAN_POINT ( 'NONE',  ( 45.74753988029933538, 116.0651871740939924, 30.44471234641811819 ) ) ;
#20722 = VERTEX_POINT ( 'NONE', #15939 ) ;
#20723 = EDGE_CURVE ( 'NONE', #19662, #16205, #849, .T. ) ;
#20724 = CARTESIAN_POINT ( 'NONE',  ( -154.5594255724347761, -178.8891397928654783, 59.16757674456785310 ) ) ;
#20725 = VERTEX_POINT ( 'NONE', #18938 ) ;
#20726 = CARTESIAN_POINT ( 'NONE',  ( 43.01140435219951286, 96.53445800887257633, 39.46799094044489209 ) ) ;
#20727 = CARTESIAN_POINT ( 'NONE',  ( 40.27526882409969744, 149.9297705074273210, 30.44471234641812174 ) ) ;
#20728 = CARTESIAN_POINT ( 'NONE',  ( 46.59305225739526435, 61.57977050742731251, 36.81289934271958941 ) ) ;
#20730 = CARTESIAN_POINT ( 'NONE',  ( 15.18239976710701100, 124.4615124019231018, 16.34704286353642999 ) ) ;
#20729 = CARTESIAN_POINT ( 'NONE',  ( 44.37947211624943833, 115.0151871740940095, 38.42115945441014446 ) ) ;
#20731 = CARTESIAN_POINT ( 'NONE',  ( 44.55648932407425633, 73.61049967264874283, 38.96596240072933170 ) ) ;
#20733 = CARTESIAN_POINT ( 'NONE',  ( 43.01140435219951996, 10.71049967264875491, 34.21067981925357060 ) ) ;
#20732 = CARTESIAN_POINT ( 'NONE',  ( 38.96631938032478359, 107.4844580088725792, 31.27175355779120025 ) ) ;
#20734 = CARTESIAN_POINT ( 'NONE',  ( -159.5594255724347761, -172.8630981290893089, 43.77915905869157598 ) ) ;
#20735 = CARTESIAN_POINT ( 'NONE',  ( 47.34993709379126159, 95.28571532017744516, 36.71770137080346785 ) ) ;
#20736 = CARTESIAN_POINT ( 'NONE',  ( 41.64333658814960870, 72.71518717409399812, 38.42115945441014446 ) ) ;
#20737 = CARTESIAN_POINT ( 'NONE',  ( 38.96631938032478359, 63.41049967264873999, 31.27175355779120025 ) ) ;
#20738 = CARTESIAN_POINT ( 'NONE',  ( -142.0420953463936087, -183.3938272943107108, 49.65701158161630957 ) ) ;
#20739 = CARTESIAN_POINT ( 'NONE',  ( -157.2955611005345986, -190.7084106276440423, 57.67623309621197336 ) ) ;
#20740 = ORIENTED_EDGE ( 'NONE', *, *, #19729, .F. ) ;
#20741 = CARTESIAN_POINT ( 'NONE',  ( -142.0420953463935803, -180.8084106276440366, 52.72008163687743831 ) ) ;
#20742 = CARTESIAN_POINT ( 'NONE',  ( 15.82680954991375621, 98.96776360684994245, 0.3584833779906905771 ) ) ;
#20743 = VERTEX_POINT ( 'NONE', #12642 ) ;
#20744 = CARTESIAN_POINT ( 'NONE',  ( 40.27526882409969033, 141.5651871740940067, 37.97664729208901946 ) ) ;
#20745 = CYLINDRICAL_SURFACE ( 'NONE', #16240, 4.999999999999997335 ) ;
#20746 = CARTESIAN_POINT ( 'NONE',  ( 47.43856463449118621, 100.8797705074273239, 34.21067981925357060 ) ) ;
#20747 = CARTESIAN_POINT ( 'NONE',  ( 48.17517050666977241, 153.7480039124125994, 4.005852979123367241 ) ) ;
#20748 = EDGE_CURVE ( 'NONE', #18561, #18469, #3838, .T. ) ;
#20749 = ORIENTED_EDGE ( 'NONE', *, *, #11554, .T. ) ;
#20750 = AXIS2_PLACEMENT_3D ( 'NONE', #14397, #12968, #4261 ) ;
#20751 = CARTESIAN_POINT ( 'NONE',  ( 63.07923660420441792, 139.7192868340247571, 4.799362114056002326 ) ) ;
#20752 = ORIENTED_EDGE ( 'NONE', *, *, #21284, .F. ) ;
#20753 = CARTESIAN_POINT ( 'NONE',  ( -91.10645082872859746, 10.96617311717548660, 4.000000000000021316 ) ) ;
#20754 = CARTESIAN_POINT ( 'NONE',  ( 39.42975644700377558, 81.67977050742732104, 36.81289934271958941 ) ) ;
#20755 = CARTESIAN_POINT ( 'NONE',  ( 44.37947211624943833, 149.2151871740940123, 30.00020018409699318 ) ) ;
#20756 = CARTESIAN_POINT ( 'NONE',  ( 41.46631938032478359, 103.3104996726487457, 38.96596240072933170 ) ) ;
#20757 = CARTESIAN_POINT ( 'NONE',  ( 57.94507594753278568, 150.7106492751291569, -2.660852849641732298 ) ) ;
#20758 = DIRECTION ( 'NONE',  ( -1.233581138472395521E-15, 0.000000000000000000, 1.000000000000000000 ) ) ;
#20759 = CARTESIAN_POINT ( 'NONE',  ( -143.3790856849358306, -172.2891397928654840, 55.53486410454105027 ) ) ;
#20760 = CARTESIAN_POINT ( 'NONE',  ( 43.01140435219951286, 152.0344580088725763, 29.21067981925356705 ) ) ;
#20761 = UNCERTAINTY_MEASURE_WITH_UNIT (LENGTH_MEASURE( 1.000000000000000082E-05 ), #14733, 'distance_accuracy_value', 'NONE');
#20762 = CARTESIAN_POINT ( 'NONE',  ( 38.96631938032478359, 144.0844580088725877, 37.14960608071593384 ) ) ;
#20763 = CARTESIAN_POINT ( 'NONE',  ( 43.01140435219951286, 113.9604996726487371, 29.21067981925356705 ) ) ;
#20764 = VECTOR ( 'NONE', #4721, 1000.000000000000000 ) ;
#20765 = EDGE_LOOP ( 'NONE', ( #19688, #13952 ) ) ;
#20766 = CARTESIAN_POINT ( 'NONE',  ( 45.74753988029933538, 83.32977050742732672, 30.44471234641811819 ) ) ;
#20767 = CARTESIAN_POINT ( 'NONE',  ( -160.8964159109769696, -166.8938272943107393, 49.65701158161630957 ) ) ;
#20768 = CARTESIAN_POINT ( 'NONE',  ( 45.74753988029934249, 76.16518717409400097, 37.97664729208901235 ) ) ;
#20769 = CARTESIAN_POINT ( 'NONE',  ( 76.81974253126139729, 125.2811442093199616, -1.589308178208348910 ) ) ;
#20770 = LINE ( 'NONE', #9415, #19565 ) ;
#20771 = VERTEX_POINT ( 'NONE', #2075 ) ;
#20772 = CARTESIAN_POINT ( 'NONE',  ( -161.4692556286852891, -175.4130981290893203, 52.90620854394536821 ) ) ;
#20773 = LINE ( 'NONE', #19012, #12035 ) ;
#20774 = CARTESIAN_POINT ( 'NONE',  ( 44.37947211624943833, 136.2797705074273154, 38.42115945441014446 ) ) ;
#20775 = CARTESIAN_POINT ( 'NONE',  ( 51.06471579629997137, 92.96554497763615643, 8.089385107838625188 ) ) ;
#20776 = ORIENTED_EDGE ( 'NONE', *, *, #9681, .T. ) ;
#20777 = CARTESIAN_POINT ( 'NONE',  ( 43.01140435219951996, 119.9070776186055838, 8.284271247461942878 ) ) ;
#20778 = ORIENTED_EDGE ( 'NONE', *, *, #15409, .T. ) ;
#20779 = CARTESIAN_POINT ( 'NONE',  ( 40.27526882409969033, 140.9297705074273210, 30.44471234641811819 ) ) ;
#20780 = AXIS2_PLACEMENT_3D ( 'NONE', #4856, #6636, #11575 ) ;
#20781 = EDGE_CURVE ( 'NONE', #17291, #4877, #8805, .T. ) ;
#20782 = DIRECTION ( 'NONE',  ( 0.000000000000000000, -1.000000000000000000, 0.000000000000000000 ) ) ;
#20783 = CARTESIAN_POINT ( 'NONE',  ( 44.55648932407425633, 120.6844580088725962, 38.96596240072933170 ) ) ;
#20784 = CARTESIAN_POINT ( 'NONE',  ( 42.21948215057683740, 159.0373810949690494, 29.21067981925356705 ) ) ;
#20785 = CARTESIAN_POINT ( 'NONE',  ( 43.01140435219951286, 93.86518717409400381, 38.86567161673127657 ) ) ;
#20786 = LINE ( 'NONE', #19553, #9776 ) ;
#20787 = FACE_OUTER_BOUND ( 'NONE', #21155, .T. ) ;
#20788 = CARTESIAN_POINT ( 'NONE',  ( -148.3790856849358306, -156.6630981290892919, 59.16757674456786020 ) ) ;
#20789 = CARTESIAN_POINT ( 'NONE',  ( 47.05648932407426344, 109.5844580088725735, 31.27175355779120025 ) ) ;
#20790 = CARTESIAN_POINT ( 'NONE',  ( 38.01140435219951996, 128.9344580088726104, 35.83527830041810347 ) ) ;
#20791 = CARTESIAN_POINT ( 'NONE',  ( 43.01140435219951286, 115.1297705074272955, 38.86567161673127657 ) ) ;
#20792 =( BOUNDED_CURVE ( )  B_SPLINE_CURVE ( 2, ( #10199, #16902, #1815, #8549, #11947, #3579, #266, #7001, #13706, #20441, #5333, #10412, #8760 ),
 .UNSPECIFIED., .F., .F. ) 
 B_SPLINE_CURVE_WITH_KNOTS ( ( 3, 2, 2, 2, 2, 2, 3 ),
 ( 0.5661764705882352811, 0.5676470588235293935, 0.5705882352941176183, 0.5735294117647058432, 0.5764705882352940680, 0.5794117647058824039, 0.5808823529411765163 ),
 .UNSPECIFIED. ) 
 CURVE ( )  GEOMETRIC_REPRESENTATION_ITEM ( )  RATIONAL_B_SPLINE_CURVE ( ( 0.9755282581475768211, 0.9755282581475768211, 1.000000000000000000, 0.9510565162951535312, 1.000000000000000000, 0.9510565162951535312, 1.000000000000000000, 0.9510565162951535312, 1.000000000000000000, 0.9510565162951535312, 1.000000000000000000, 0.9755282581475768211, 0.9755282581475768211 ) ) 
 REPRESENTATION_ITEM ( '' )  );
#20793 = CARTESIAN_POINT ( 'NONE',  ( 43.17520790721623314, 91.62706341066298421, 13.41396976009479403 ) ) ;
#20794 = CARTESIAN_POINT ( 'NONE',  ( -142.0420953463935803, -195.2438272943107336, 46.59394152635518793 ) ) ;
#20795 = CARTESIAN_POINT ( 'NONE',  ( 47.43856463449117911, 103.7651871740939669, 32.77220824515697473 ) ) ;
#20796 = CARTESIAN_POINT ( 'NONE',  ( -141.4692556286852891, -162.2130981290893033, 52.90620854394536821 ) ) ;
#20797 = ORIENTED_EDGE ( 'NONE', *, *, #18850, .T. ) ;
#20798 = CARTESIAN_POINT ( 'NONE',  ( 39.92123440845005433, 88.16049967264873999, 38.46393386101375711 ) ) ;
#20799 = EDGE_CURVE ( 'NONE', #1989, #21208, #7859, .T. ) ;
#20800 = CARTESIAN_POINT ( 'NONE',  ( 32.31036143884366396, 152.4250368413922274, -10.51794503956956817 ) ) ;
#20801 = CARTESIAN_POINT ( 'NONE',  ( 19.52755003174225124, 104.2962547294809070, 15.51356631106660089 ) ) ;
#20802 = CARTESIAN_POINT ( 'NONE',  ( 43.01140435219951996, 10.71049967264875491, 34.21067981925357060 ) ) ;
#20803 = EDGE_CURVE ( 'NONE', #7232, #10397, #21572, .T. ) ;
#20804 = CARTESIAN_POINT ( 'NONE',  ( 38.58424406990785371, 72.52977050742731535, 35.64915139335015937 ) ) ;
#20805 = ORIENTED_EDGE ( 'NONE', *, *, #1282, .T. ) ;
#20806 = ADVANCED_FACE ( 'NONE', ( #13076 ), #1395, .T. ) ;
#20807 = ORIENTED_EDGE ( 'NONE', *, *, #20038, .F. ) ;
#20808 = CARTESIAN_POINT ( 'NONE',  ( 44.55648932407425633, 60.68445800887258201, 38.96596240072933170 ) ) ;
#20809 = FACE_BOUND ( 'NONE', #4015, .T. ) ;
#20810 = EDGE_CURVE ( 'NONE', #21725, #14883, #2602, .T. ) ;
#20811 = CARTESIAN_POINT ( 'NONE',  ( 43.01140435219951286, 116.9604996726487514, 28.95336869806222779 ) ) ;
#20813 = CARTESIAN_POINT ( 'NONE',  ( 61.89860894053757789, 148.3622700476249463, -1.513601781051955530 ) ) ;
#20812 = CARTESIAN_POINT ( 'NONE',  ( 40.27526882409969033, 78.56518717409399244, 37.97664729208901946 ) ) ;
#20814 = CARTESIAN_POINT ( 'NONE',  ( -145.6429501568359797, -183.8438272943107279, 57.67623309621197336 ) ) ;
#20815 = CARTESIAN_POINT ( 'NONE',  ( 48.01140435219951996, 113.3604996726487286, 32.58608133808903773 ) ) ;
#20816 = CARTESIAN_POINT ( 'NONE',  ( -145.2889157411863721, -185.6130981290892805, 41.15050349809590102 ) ) ;
#20817 = CARTESIAN_POINT ( 'NONE',  ( 43.80332655382220253, 67.53738109496899256, 39.21067981925355639 ) ) ;
#20818 = CARTESIAN_POINT ( 'NONE',  ( -141.4692556286852891, -163.1391397928654783, 52.90620854394536821 ) ) ;
#20819 = CARTESIAN_POINT ( 'NONE',  ( 38.58424406990786082, 144.3797705074273097, 34.21067981925357060 ) ) ;
#20820 = CARTESIAN_POINT ( 'NONE',  ( 51.15470623622070434, 86.57325545146775880, 6.072769092256255163 ) ) ;
#20821 = CARTESIAN_POINT ( 'NONE',  ( 38.58424406990785371, 131.9651871740939839, 32.77220824515697473 ) ) ;
#20822 = CARTESIAN_POINT ( 'NONE',  ( -155.3247640818418063, -155.4453048272798412, 40.99743929837026712 ) ) ;
#20823 = CARTESIAN_POINT ( 'NONE',  ( -160.8964159109769696, -170.1584106276440593, 49.65701158161630957 ) ) ;
#20824 = EDGE_CURVE ( 'NONE', #6019, #18253, #2935, .T. ) ;
#20825 = LINE ( 'NONE', #10795, #8688 ) ;
#20826 = CARTESIAN_POINT ( 'NONE',  ( 26.22827968769296092, 97.14409021710402214, 14.12817222279094942 ) ) ;
#20827 = CARTESIAN_POINT ( 'NONE',  ( 33.01140435219951286, 119.9070776186055838, -35.00000000000000000 ) ) ;
#20828 = CARTESIAN_POINT ( 'NONE',  ( 41.64333658814960870, 114.7151871740940123, 38.42115945441014446 ) ) ;
#20829 = EDGE_CURVE ( 'NONE', #15960, #20168, #16267, .T. ) ;
#20830 = ORIENTED_EDGE ( 'NONE', *, *, #20803, .T. ) ;
#20831 = DIRECTION ( 'NONE',  ( 0.9393725726208708160, 0.3428981916074316239, -0.000000000000000000 ) ) ;
#20832 = ORIENTED_EDGE ( 'NONE', *, *, #13923, .T. ) ;
#20833 = CARTESIAN_POINT ( 'NONE',  ( 39.92123440845004723, 89.33445800887257349, 29.95742577749337343 ) ) ;
#20834 = CARTESIAN_POINT ( 'NONE',  ( 44.37947211624943833, 149.4797705074273324, 30.00020018409699318 ) ) ;
#20835 = AXIS2_PLACEMENT_3D ( 'NONE', #15587, #10745, #5549 ) ;
#20836 = CARTESIAN_POINT ( 'NONE',  ( 41.46631938032478359, 150.1104996726487570, 29.45539723777780239 ) ) ;
#20838 = CARTESIAN_POINT ( 'NONE',  ( 17.65293208513390866, 132.0582047407114885, -3.339186312533837242 ) ) ;
#20837 = CARTESIAN_POINT ( 'NONE',  ( 38.58424406990784661, 105.2651871740939953, 35.64915139335016647 ) ) ;
#20839 = CARTESIAN_POINT ( 'NONE',  ( 48.01140435219951996, 74.06049967264874567, 35.83527830041810347 ) ) ;
#20840 = CARTESIAN_POINT ( 'NONE',  ( -161.4692556286852891, -157.4130981290893203, 52.90620854394536821 ) ) ;
#20841 = CARTESIAN_POINT ( 'NONE',  ( 47.05648932407426344, 118.5844580088725735, 31.27175355779120025 ) ) ;
#20842 = VECTOR ( 'NONE', #4238, 1000.000000000000000 ) ;
#20843 = CARTESIAN_POINT ( 'NONE',  ( 38.96631938032478359, 71.48445800887257917, 31.27175355779120025 ) ) ;
#20844 = CARTESIAN_POINT ( 'NONE',  ( 72.34521997529867576, 314.8592298662555322, -4.000000000000003553 ) ) ;
#20845 = CARTESIAN_POINT ( 'NONE',  ( 47.43856463449117200, 67.46518717409399812, 35.64915139335016647 ) ) ;
#20846 = CARTESIAN_POINT ( 'NONE',  ( 43.01140435219951286, 62.96049967264873004, 29.21067981925356705 ) ) ;
#20847 = CARTESIAN_POINT ( 'NONE',  ( -143.8425227516148084, -177.6938272943107506, 55.19815736654470584 ) ) ;
#20848 = CARTESIAN_POINT ( 'NONE',  ( 96.62434152388762243, 220.7958015105191976, -5.999999999999976019 ) ) ;
#20849 = ORIENTED_EDGE ( 'NONE', *, *, #12606, .T. ) ;
#20850 = CARTESIAN_POINT ( 'NONE',  ( -143.8425227516148084, -174.9584106276440707, 55.19815736654470584 ) ) ;
#20851 = CARTESIAN_POINT ( 'NONE',  ( 61.62447910614003632, 148.7338836329059859, 10.47761036752830144 ) ) ;
#20852 = CARTESIAN_POINT ( 'NONE',  ( -151.4692556286852891, -196.9891397928655010, 49.65701158161630957 ) ) ;
#20853 = AXIS2_PLACEMENT_3D ( 'NONE', #1304, #9694, #1194 ) ;
#20854 = CARTESIAN_POINT ( 'NONE',  ( 40.27526882409969033, 140.6651871740939725, 30.44471234641811819 ) ) ;
#20855 = CARTESIAN_POINT ( 'NONE',  ( 40.27526882409969744, 107.9297705074273352, 30.44471234641812174 ) ) ;
#20856 = VERTEX_POINT ( 'NONE', #18136 ) ;
#20857 = VERTEX_POINT ( 'NONE', #1173 ) ;
#20858 = AXIS2_PLACEMENT_3D ( 'NONE', #9759, #18232, #19447 ) ;
#20859 = CARTESIAN_POINT ( 'NONE',  ( 18.57470074671828542, 105.8336742703428257, 1.585105279193314010 ) ) ;
#20860 = EDGE_LOOP ( 'NONE', ( #3231, #13934, #17400, #17697 ) ) ;
#20861 = CARTESIAN_POINT ( 'NONE',  ( 38.96631938032478359, 116.4844580088725792, 31.27175355779120025 ) ) ;
#20862 = CARTESIAN_POINT ( 'NONE',  ( 44.55648932407425633, 89.81049967264874567, 29.45539723777780239 ) ) ;
#20863 = CARTESIAN_POINT ( 'NONE',  ( 41.64333658814960870, 83.77977050742732956, 30.00020018409699318 ) ) ;
#20864 = CARTESIAN_POINT ( 'NONE',  ( 38.58424406990784661, 138.2651871740939669, 35.64915139335016647 ) ) ;
#20865 = CARTESIAN_POINT ( 'NONE',  ( 38.01140435219951996, 102.5604996726487599, 32.58608133808903773 ) ) ;
#20866 = CARTESIAN_POINT ( 'NONE',  ( 26.28921445626723852, 149.7786157371718616, -3.732453678475698311 ) ) ;
#20867 = CARTESIAN_POINT ( 'NONE',  ( -149.8854112254399240, -180.7362167067690280, 59.65701158161632378 ) ) ;
#20868 = CARTESIAN_POINT ( 'NONE',  ( -148.3790856849358306, -172.5891397928654669, 59.16757674456786020 ) ) ;
#20869 = CARTESIAN_POINT ( 'NONE',  ( -151.4692556286852607, -161.3130981290892976, 39.65701158161629536 ) ) ;
#20870 = EDGE_CURVE ( 'NONE', #1227, #14246, #4582, .T. ) ;
#20871 = CARTESIAN_POINT ( 'NONE',  ( 46.10157429594899270, 64.73445800887257917, 29.95742577749336988 ) ) ;
#20872 = CARTESIAN_POINT ( 'NONE',  ( 43.01140435219951286, 105.5344580088725621, 39.21067981925356349 ) ) ;
#20873 = ORIENTED_EDGE ( 'NONE', *, *, #1561, .T. ) ;
#20874 = CARTESIAN_POINT ( 'NONE',  ( 43.01140435219951286, 85.12977050742729546, 38.86567161673127657 ) ) ;
#20875 = CARTESIAN_POINT ( 'NONE',  ( -157.2955611005346270, -164.3438272943107279, 41.63779006702063867 ) ) ;
#20876 = CARTESIAN_POINT ( 'NONE',  ( 40.27526882409969744, 66.56518717409400665, 37.97664729208901235 ) ) ;
#20877 = CARTESIAN_POINT ( 'NONE',  ( 73.32203938827501588, 103.9946350594383517, -0.8753108214479579097 ) ) ;
#20878 = CARTESIAN_POINT ( 'NONE',  ( -143.8425227516148084, -192.3584106276440480, 44.11586579668791330 ) ) ;
#20879 = ORIENTED_EDGE ( 'NONE', *, *, #4244, .T. ) ;
#20880 = CARTESIAN_POINT ( 'NONE',  ( -157.6495955161842062, -176.0130981290893146, 41.15050349809589392 ) ) ;
#20881 = LINE ( 'NONE', #4330, #16952 ) ;
#20882 = CARTESIAN_POINT ( 'NONE',  ( 41.64333658814960870, 129.9797705074273040, 38.42115945441014446 ) ) ;
#20883 = CARTESIAN_POINT ( 'NONE',  ( 23.45433402446531446, 147.8217840461813068, -16.84717431919864339 ) ) ;
#20884 = ORIENTED_EDGE ( 'NONE', *, *, #17887, .T. ) ;
#20885 = CARTESIAN_POINT ( 'NONE',  ( 48.01140435219951996, 73.43445800887256780, 32.58608133808903773 ) ) ;
#20886 = ORIENTED_EDGE ( 'NONE', *, *, #11233, .T. ) ;
#20887 = CARTESIAN_POINT ( 'NONE',  ( 47.43856463449117200, 131.0297705074272869, 32.77220824515698183 ) ) ;
#20888 = CARTESIAN_POINT ( 'NONE',  ( 48.01140435219951996, 145.1344580088725991, 35.83527830041809636 ) ) ;
#20889 = CARTESIAN_POINT ( 'NONE',  ( 43.80332655382220253, 154.5373810949690210, 39.21067981925354218 ) ) ;
#20890 = CARTESIAN_POINT ( 'NONE',  ( 38.96631938032478359, 110.4844580088725792, 31.27175355779120025 ) ) ;
#20891 = PLANE ( 'NONE',  #9240 ) ;
#20892 = CARTESIAN_POINT ( 'NONE',  ( 39.92123440845005433, 159.2604996726487343, 29.95742577749336988 ) ) ;
#20893 = CARTESIAN_POINT ( 'NONE',  ( 44.37947211624943833, 97.01518717409400949, 38.42115945441014446 ) ) ;
#20894 = LINE ( 'NONE', #12512, #2024 ) ;
#20895 = CARTESIAN_POINT ( 'NONE',  ( 43.01140435219951286, 78.53445800887259054, 39.21067981925356349 ) ) ;
#20896 = CARTESIAN_POINT ( 'NONE',  ( -157.6495955161842062, -160.1130981290893089, 58.16351966513671812 ) ) ;
#20897 = PRODUCT_CONTEXT ( 'NONE', #10431, 'mechanical' ) ;
#20898 = DIRECTION ( 'NONE',  ( -0.000000000000000000, 1.000000000000000000, -0.000000000000000000 ) ) ;
#20899 = CARTESIAN_POINT ( 'NONE',  ( 38.01140435219952707, 134.7844580088726048, 34.21067981925357060 ) ) ;
#20900 = CARTESIAN_POINT ( 'NONE',  ( 38.58424406990786082, 111.3797705074273239, 34.21067981925357060 ) ) ;
#20901 = CARTESIAN_POINT ( 'NONE',  ( 18.74235739206972085, 134.4262906160203386, 8.771002148563594503 ) ) ;
#20902 = CARTESIAN_POINT ( 'NONE',  ( 43.01140435219951286, 67.46049967264873715, 39.21067981925356349 ) ) ;
#20903 = CARTESIAN_POINT ( 'NONE',  ( 47.43856463449118621, 100.6151871740940180, 34.21067981925357060 ) ) ;
#20904 = CARTESIAN_POINT ( 'NONE',  ( -143.3790856849358306, -162.3630981290893089, 55.53486410454105027 ) ) ;
#20905 = ORIENTED_EDGE ( 'NONE', *, *, #7540, .F. ) ;
#20906 = CARTESIAN_POINT ( 'NONE',  ( 33.01140435219951286, 119.9070776186055838, -19.99999999999998579 ) ) ;
#20907 = EDGE_CURVE ( 'NONE', #4859, #18638, #11302, .T. ) ;
#20908 = CARTESIAN_POINT ( 'NONE',  ( 75.10802748102119608, 108.0013139708956800, -8.018167963582932600 ) ) ;
#20909 = CARTESIAN_POINT ( 'NONE',  ( 41.83412315030695794, 148.0818998446914634, 10.87053871734362431 ) ) ;
#20910 = CARTESIAN_POINT ( 'NONE',  ( -145.2889157411863437, -168.5391397928654840, 41.15050349809589392 ) ) ;
#20911 = VECTOR ( 'NONE', #17689, 1000.000000000000000 ) ;
#20912 = CARTESIAN_POINT ( 'NONE',  ( 40.27526882409969744, 71.92977050742729261, 30.44471234641812174 ) ) ;
#20913 = EDGE_LOOP ( 'NONE', ( #2330, #20886, #10536, #16469 ) ) ;
#20914 = ORIENTED_EDGE ( 'NONE', *, *, #16678, .T. ) ;
#20915 = PRODUCT_DEFINITION ( 'UNKNOWN', '', #3886, #10389 ) ;
#20916 = DIRECTION ( 'NONE',  ( -0.000000000000000000, -0.000000000000000000, 1.000000000000000000 ) ) ;
#20917 = AXIS2_PLACEMENT_3D ( 'NONE', #10469, #1865, #7379 ) ;
#20919 = EDGE_CURVE ( 'NONE', #6406, #5105, #13183, .T. ) ;
#20918 = CARTESIAN_POINT ( 'NONE',  ( 38.96631938032478359, 121.0104996726487343, 37.14960608071593384 ) ) ;
#20921 = CARTESIAN_POINT ( 'NONE',  ( 77.09984031027478579, 117.8059907461747429, -7.347010041119995449 ) ) ;
#20920 = CARTESIAN_POINT ( 'NONE',  ( 38.58424406990786082, 81.11518717409398960, 34.21067981925357060 ) ) ;
#20922 =( BOUNDED_CURVE ( )  B_SPLINE_CURVE ( 2, ( #20089, #11799, #12446, #15538, #7288, #14096, #18961, #10587, #4073, #10802, #3972, #8832, #17507 ),
 .UNSPECIFIED., .F., .F. ) 
 B_SPLINE_CURVE_WITH_KNOTS ( ( 3, 2, 2, 2, 2, 2, 3 ),
 ( 0.8035714285714286031, 0.8071428571428571619, 0.8142857142857142794, 0.8214285714285713969, 0.8285714285714286254, 0.8357142857142857428, 0.8392857142857143016 ),
 .UNSPECIFIED. ) 
 CURVE ( )  GEOMETRIC_REPRESENTATION_ITEM ( )  RATIONAL_B_SPLINE_CURVE ( ( 0.9755282581475768211, 0.9755282581475768211, 1.000000000000000000, 0.9510565162951535312, 1.000000000000000000, 0.9510565162951535312, 1.000000000000000000, 0.9510565162951535312, 1.000000000000000000, 0.9510565162951535312, 1.000000000000000000, 0.9755282581475768211, 0.9755282581475768211 ) ) 
 REPRESENTATION_ITEM ( '' )  );
#20923 = CARTESIAN_POINT ( 'NONE',  ( -142.0420953463935803, -171.2438272943107052, 46.59394152635518083 ) ) ;
#20924 = CARTESIAN_POINT ( 'NONE',  ( 65.27013532398795803, 145.9152199903044504, 11.62486143609835310 ) ) ;
#20925 = CARTESIAN_POINT ( 'NONE',  ( -143.3790856849358306, -186.3630981290893089, 55.53486410454105027 ) ) ;
#20926 =( LENGTH_UNIT ( ) NAMED_UNIT ( * ) SI_UNIT ( .MILLI., .METRE. ) );
#20927 = DIRECTION ( 'NONE',  ( -1.000000000000000000, 0.000000000000000000, 0.000000000000000000 ) ) ;
#20928 = FACE_OUTER_BOUND ( 'NONE', #5221, .T. ) ;
#20929 = CARTESIAN_POINT ( 'NONE',  ( 38.58424406990784661, 138.2297705074273324, 32.77220824515698183 ) ) ;
#20930 = EDGE_CURVE ( 'NONE', #1138, #17533, #9671, .T. ) ;
#20931 = CARTESIAN_POINT ( 'NONE',  ( 57.78537588620154963, 150.8774031240512272, 3.334753224648476788 ) ) ;
#20932 = CARTESIAN_POINT ( 'NONE',  ( 40.27526882409969744, 135.5651871740940067, 37.97664729208901235 ) ) ;
#20933 = CARTESIAN_POINT ( 'NONE',  ( 44.55648932407425633, 137.8104996726487457, 29.45539723777780239 ) ) ;
#20934 = CARTESIAN_POINT ( 'NONE',  ( -145.6429501568359797, -166.1084106276440195, 57.67623309621197336 ) ) ;
#20935 = CARTESIAN_POINT ( 'NONE',  ( -153.0531000319307111, -165.1622583705451746, 39.65701158161631668 ) ) ;
#20936 = CARTESIAN_POINT ( 'NONE',  ( 18.01140435219953062, 119.9070776186055838, 50.00000000000002842 ) ) ;
#20937 = VECTOR ( 'NONE', #20327, 1000.000000000000000 ) ;
#20938 = CARTESIAN_POINT ( 'NONE',  ( 69.40534582624466964, 109.7482951092767678, 5.080680574306066788 ) ) ;
#20939 = CARTESIAN_POINT ( 'NONE',  ( 41.64333658814960870, 102.7151871740939981, 38.42115945441014446 ) ) ;
#20940 = COLOUR_RGB ( '', 0.66274510, 0.83137255, 0.94901961) ;
#20941 = EDGE_LOOP ( 'NONE', ( #683, #14556 ) ) ;
#20942 = DIRECTION ( 'NONE',  ( 0.000000000000000000, 1.000000000000000000, 0.000000000000000000 ) ) ;
#20943 = ORIENTED_EDGE ( 'NONE', *, *, #712, .T. ) ;
#20944 = CARTESIAN_POINT ( 'NONE',  ( 41.46631938032478359, 96.38445800887257064, 38.96596240072933170 ) ) ;
#20945 = CARTESIAN_POINT ( 'NONE',  ( 38.01140435219951996, 144.8604996726487002, 35.83527830041810347 ) ) ;
#20947 = CARTESIAN_POINT ( 'NONE',  ( 29.44877014884911404, 144.5398477306827942, -9.648498702473171207 ) ) ;
#20946 = CARTESIAN_POINT ( 'NONE',  ( 38.58424406990786082, 108.1151871740940038, 34.21067981925357060 ) ) ;
#20948 = CARTESIAN_POINT ( 'NONE',  ( 48.01140435219951996, 62.21049967264874425, 34.21067981925357060 ) ) ;
#20950 = DIRECTION ( 'NONE',  ( 0.000000000000000000, -1.000000000000000000, 0.000000000000000000 ) ) ;
#20949 = CARTESIAN_POINT ( 'NONE',  ( 46.77338793169477782, 144.6226297781437324, 37.50829531803061911 ) ) ;
#20951 = DIRECTION ( 'NONE',  ( 0.000000000000000000, 1.000000000000000000, 0.000000000000000000 ) ) ;
#20952 = DIRECTION ( 'NONE',  ( 0.000000000000000000, 0.000000000000000000, 1.000000000000000000 ) ) ;
#20953 = DIRECTION ( 'NONE',  ( 1.000000000000000000, 0.000000000000000000, 0.000000000000000000 ) ) ;
#20954 = CARTESIAN_POINT ( 'NONE',  ( 38.58424406990786082, 66.11518717409398960, 34.21067981925357060 ) ) ;
#20955 = CARTESIAN_POINT ( 'NONE',  ( 145.5008360144876747, 198.5836349573982886, 34.00000000000001421 ) ) ;
#20956 = CARTESIAN_POINT ( 'NONE',  ( 32.23767430054684979, 145.5917660130465379, 17.43780275515692679 ) ) ;
#20957 = AXIS2_PLACEMENT_3D ( 'NONE', #2841, #14417, #1192 ) ;
#20958 = CARTESIAN_POINT ( 'NONE',  ( -142.0420953463936087, -171.3938272943107393, 49.65701158161630957 ) ) ;
#20959 = CARTESIAN_POINT ( 'NONE',  ( -160.8964159109769696, -191.1584106276440593, 49.65701158161630957 ) ) ;
#20960 = ORIENTED_EDGE ( 'NONE', *, *, #6074, .F. ) ;
#20961 = CARTESIAN_POINT ( 'NONE',  ( -143.8425227516148084, -180.3584106276440480, 44.11586579668791330 ) ) ;
#20962 = CARTESIAN_POINT ( 'NONE',  ( 9.529548018246485341, 127.4200721877477491, 8.334841288026581196 ) ) ;
#20963 = DIRECTION ( 'NONE',  ( 0.000000000000000000, 1.000000000000000000, 0.000000000000000000 ) ) ;
#20964 = CARTESIAN_POINT ( 'NONE',  ( 44.37947211624943833, 140.2151871740940123, 30.00020018409699318 ) ) ;
#20965 = CARTESIAN_POINT ( 'NONE',  ( 46.59305225739526435, 103.5797705074273267, 36.81289934271958941 ) ) ;
#20966 = EDGE_LOOP ( 'NONE', ( #16095, #10769 ) ) ;
#20967 = ORIENTED_EDGE ( 'NONE', *, *, #8565, .T. ) ;
#20968 = CARTESIAN_POINT ( 'NONE',  ( 29.12819380265916180, 95.36133955912156068, 0.9897074016940036190 ) ) ;
#20969 = VERTEX_POINT ( 'NONE', #8018 ) ;
#20970 = CARTESIAN_POINT ( 'NONE',  ( 173.3794444120442506, -34.13255853780189142, 20.00000000000001776 ) ) ;
#20971 = VECTOR ( 'NONE', #8326, 1000.000000000000000 ) ;
#20972 = ADVANCED_FACE ( 'NONE', ( #19470 ), #14610, .T. ) ;
#20973 = CARTESIAN_POINT ( 'NONE',  ( 47.43856463449117200, 76.72977050742733240, 35.64915139335016647 ) ) ;
#20974 = CARTESIAN_POINT ( 'NONE',  ( 44.37947211624943833, 136.0151871740939953, 38.42115945441014446 ) ) ;
#20975 = CARTESIAN_POINT ( 'NONE',  ( 47.05648932407426344, 98.51049967264874851, 31.27175355779120025 ) ) ;
#20976 = CARTESIAN_POINT ( 'NONE',  ( 42.92180000979148957, 85.67454126555050209, 7.339147150375312734 ) ) ;
#20977 = CARTESIAN_POINT ( 'NONE',  ( 40.79866406026947345, 95.00477161731822662, 29.72396354041403299 ) ) ;
#20978 = CARTESIAN_POINT ( 'NONE',  ( -148.3790856849358306, -157.5891397928654953, 59.16757674456786020 ) ) ;
#20979 = DIRECTION ( 'NONE',  ( -2.779543948608941985E-16, 1.000000000000000000, 0.000000000000000000 ) ) ;
#20980 = FACE_OUTER_BOUND ( 'NONE', #4829, .T. ) ;
#20981 =( REPRESENTATION_RELATIONSHIP ('NONE','NONE', #6933, #15921 ) REPRESENTATION_RELATIONSHIP_WITH_TRANSFORMATION ( #3478 )SHAPE_REPRESENTATION_RELATIONSHIP( ) );
#20982 = DIRECTION ( 'NONE',  ( -0.8660254037844384856, 0.000000000000000000, -0.5000000000000003331 ) ) ;
#20983 = CIRCLE ( 'NONE', #5417, 14.42424326798555434 ) ;
#20984 = VECTOR ( 'NONE', #17228, 1000.000000000000000 ) ;
#20985 = VERTEX_POINT ( 'NONE', #18028 ) ;
#20986 = CARTESIAN_POINT ( 'NONE',  ( 41.64333658814960870, 86.77977050742731535, 30.00020018409699318 ) ) ;
#20987 = CARTESIAN_POINT ( 'NONE',  ( -142.0420953463936087, -168.3938272943107393, 49.65701158161630957 ) ) ;
#20988 = CARTESIAN_POINT ( 'NONE',  ( 32.98198692859195802, 152.6383102900375093, -3.493975233523312962 ) ) ;
#20989 = CARTESIAN_POINT ( 'NONE',  ( -157.2955611005346270, -190.7084106276440423, 57.67623309621198047 ) ) ;
#20990 = ORIENTED_EDGE ( 'NONE', *, *, #15409, .F. ) ;
#20991 = CARTESIAN_POINT ( 'NONE',  ( 44.55648932407425633, 85.88445800887258486, 29.45539723777780239 ) ) ;
#20992 = CYLINDRICAL_SURFACE ( 'NONE', #2527, 10.00000000000000888 ) ;
#20993 = CARTESIAN_POINT ( 'NONE',  ( 43.01140435219951286, 137.6297705074273381, 29.55568802177586107 ) ) ;
#20994 = CARTESIAN_POINT ( 'NONE',  ( 26.51748177580332566, 149.8140053266110385, -9.728054792207391444 ) ) ;
#20995 = ORIENTED_EDGE ( 'NONE', *, *, #20829, .F. ) ;
#20996 = CARTESIAN_POINT ( 'NONE',  ( 46.10157429594899270, 73.73445800887256496, 29.95742577749336988 ) ) ;
#20997 = ORIENTED_EDGE ( 'NONE', *, *, #12332, .F. ) ;
#20998 = CARTESIAN_POINT ( 'NONE',  ( 40.27526882409969033, 125.9297705074273352, 30.44471234641811819 ) ) ;
#20999 = CARTESIAN_POINT ( 'NONE',  ( 43.80332655382221674, 133.5373810949689926, 39.21067981925355639 ) ) ;
#21000 = EDGE_CURVE ( 'NONE', #8015, #16997, #7369, .T. ) ;
#21001 = CARTESIAN_POINT ( 'NONE',  ( 47.43856463449118621, 88.87977050742732388, 34.21067981925357060 ) ) ;
#21002 = CIRCLE ( 'NONE', #17118, 10.00000000000000888 ) ;
#21003 = DIRECTION ( 'NONE',  ( -0.5250363069212118372, 0.8510798296367592108, 0.000000000000000000 ) ) ;
#21004 = CARTESIAN_POINT ( 'NONE',  ( -176.9699209214867608, 160.7104996726487514, -35.00000000000000000 ) ) ;
#21005 = CARTESIAN_POINT ( 'NONE',  ( 38.01140435219952707, 159.5604996726487457, 32.58608133808903773 ) ) ;
#21006 = CARTESIAN_POINT ( 'NONE',  ( -159.5594255724347761, -194.1891397928654897, 55.53486410454104316 ) ) ;
#21007 = CARTESIAN_POINT ( 'NONE',  ( 38.58424406990786082, 90.11518717409400381, 34.21067981925357060 ) ) ;
#21008 = DIRECTION ( 'NONE',  ( 0.000000000000000000, 0.000000000000000000, -1.000000000000000000 ) ) ;
#21009 = DIRECTION ( 'NONE',  ( 0.000000000000000000, 1.000000000000000000, -0.000000000000000000 ) ) ;
#21010 = CARTESIAN_POINT ( 'NONE',  ( -148.3790856849358306, -162.6630981290892919, 59.16757674456786020 ) ) ;
#21011 = DIRECTION ( 'NONE',  ( 1.000000000000000000, 0.000000000000000000, 0.000000000000000000 ) ) ;
#21012 = CARTESIAN_POINT ( 'NONE',  ( 38.01140435219952707, 131.7844580088725763, 34.21067981925357060 ) ) ;
#21013 = CARTESIAN_POINT ( 'NONE',  ( 38.96631938032478359, 132.0844580088725877, 37.14960608071593384 ) ) ;
#21014 = CARTESIAN_POINT ( 'NONE',  ( 43.01140435219951286, 113.6297705074273097, 29.55568802177586463 ) ) ;
#21015 = CARTESIAN_POINT ( 'NONE',  ( 55.65775942066846937, 145.2030105016711445, 10.43785198868815023 ) ) ;
#21016 = CARTESIAN_POINT ( 'NONE',  ( -143.8425227516148084, -189.0938272943107279, 44.11586579668791330 ) ) ;
#21017 = CARTESIAN_POINT ( 'NONE',  ( 40.27526882409969744, 101.6651871740940010, 30.44471234641812174 ) ) ;
#21018 = CARTESIAN_POINT ( 'NONE',  ( 38.01140435219952707, 90.71049967264873715, 34.21067981925357060 ) ) ;
#21019 = EDGE_LOOP ( 'NONE', ( #21108, #13321 ) ) ;
#21020 = LINE ( 'NONE', #10770, #632 ) ;
#21021 = CARTESIAN_POINT ( 'NONE',  ( 9.468627745026951814, 113.0646104733145592, 1.862908727141013854 ) ) ;
#21022 = AXIS2_PLACEMENT_3D ( 'NONE', #14429, #17515, #17839 ) ;
#21023 = CARTESIAN_POINT ( 'NONE',  ( 52.77336176550079472, 93.53620953014643646, -12.98192714454240182 ) ) ;
#21024 = PRODUCT_DEFINITION_SHAPE ( 'NONE', 'NONE',  #21187 ) ;
#21025 = CARTESIAN_POINT ( 'NONE',  ( -148.3790856849358306, -168.3891397928654499, 40.14644641866477315 ) ) ;
#21026 = CARTESIAN_POINT ( 'NONE',  ( 39.42975644700377558, 75.07977050742731251, 31.60846029578754468 ) ) ;
#21027 = ORIENTED_EDGE ( 'NONE', *, *, #3684, .T. ) ;
#21028 = VERTEX_POINT ( 'NONE', #4694 ) ;
#21029 = CARTESIAN_POINT ( 'NONE',  ( 44.37947211624943833, 154.2797705074273438, 38.42115945441014446 ) ) ;
#21030 = CARTESIAN_POINT ( 'NONE',  ( -151.4692556286852891, -196.9891397928655010, 39.65701158161630246 ) ) ;
#21031 = CARTESIAN_POINT ( 'NONE',  ( 38.96631938032478359, 124.0104996726487343, 37.14960608071593384 ) ) ;
#21033 = CARTESIAN_POINT ( 'NONE',  ( 9.953047844039691228, 128.4882722429139505, 3.367556520687803090 ) ) ;
#21032 = CARTESIAN_POINT ( 'NONE',  ( 46.59305225739526435, 73.31518717409400665, 36.81289934271958941 ) ) ;
#21034 = AXIS2_PLACEMENT_3D ( 'NONE', #12181, #7025, #8675 ) ;
#21035 = CARTESIAN_POINT ( 'NONE',  ( -157.2955611005345986, -172.4438272943107222, 57.67623309621197336 ) ) ;
#21036 = CARTESIAN_POINT ( 'NONE',  ( 43.01140435219951286, 113.9604996726487371, 29.21067981925356705 ) ) ;
#21037 = CARTESIAN_POINT ( 'NONE',  ( -143.3790856849358306, -183.3630981290893374, 55.53486410454105027 ) ) ;
#21038 = DIRECTION ( 'NONE',  ( 0.9387810623359078566, 0.3426822732243069436, 0.03548206049944095664 ) ) ;
#21039 = CARTESIAN_POINT ( 'NONE',  ( 43.01140435219951286, 156.5344580088725763, 39.46799094044489209 ) ) ;
#21040 = CARTESIAN_POINT ( 'NONE',  ( 44.37947211624943833, 143.4797705074273324, 30.00020018409699318 ) ) ;
#21041 = CARTESIAN_POINT ( 'NONE',  ( 47.27474595639033339, 153.9548969447091906, 2.977729283044022957 ) ) ;
#21042 = CARTESIAN_POINT ( 'NONE',  ( 44.37947211624943833, 125.2151871740939981, 30.00020018409699318 ) ) ;
#21043 = CARTESIAN_POINT ( 'NONE',  ( 38.01140435219952707, 69.71049967264873715, 34.21067981925357060 ) ) ;
#21044 = CARTESIAN_POINT ( 'NONE',  ( -145.6429501568359797, -160.1084106276440480, 57.67623309621197336 ) ) ;
#21045 = CARTESIAN_POINT ( 'NONE',  ( -94.10404323627655288, -13.18023274290474767, -19.99999999999997868 ) ) ;
#21046 = ADVANCED_FACE ( 'NONE', ( #1068 ), #16043, .F. ) ;
#21047 = DIRECTION ( 'NONE',  ( -0.000000000000000000, 0.000000000000000000, -1.000000000000000000 ) ) ;
#21048 = CARTESIAN_POINT ( 'NONE',  ( 18.74235739206972085, 134.4262906160203386, 8.771002148563594503 ) ) ;
#21049 = AXIS2_PLACEMENT_3D ( 'NONE', #8113, #16470, #14819 ) ;
#21050 = CARTESIAN_POINT ( 'NONE',  ( 38.01140435219952707, 120.5604996726487457, 32.58608133808903773 ) ) ;
#21051 = CARTESIAN_POINT ( 'NONE',  ( 44.37947211624943833, 109.0151871740940095, 38.42115945441014446 ) ) ;
#21052 = VERTEX_POINT ( 'NONE', #11090 ) ;
#21053 = VECTOR ( 'NONE', #9762, 1000.000000000000000 ) ;
#21054 = CARTESIAN_POINT ( 'NONE',  ( 43.01140435219951286, 116.9604996726487371, 29.21067981925356705 ) ) ;
#21055 = ORIENTED_EDGE ( 'NONE', *, *, #13773, .F. ) ;
#21056 =( BOUNDED_CURVE ( )  B_SPLINE_CURVE ( 2, ( #1099, #2854, #9165, #6155, #777, #4393, #7512, #19611, #7619, #9490, #7834, #5944, #21277 ),
 .UNSPECIFIED., .F., .T. ) 
 B_SPLINE_CURVE_WITH_KNOTS ( ( 3, 2, 2, 2, 2, 2, 3 ),
 ( 0.2678571428571428492, 0.2714285714285714080, 0.2785714285714285809, 0.2857142857142856984, 0.2928571428571428714, 0.2999999999999999889, 0.3035714285714286031 ),
 .UNSPECIFIED. ) 
 CURVE ( )  GEOMETRIC_REPRESENTATION_ITEM ( )  RATIONAL_B_SPLINE_CURVE ( ( 0.9755282581475768211, 0.9755282581475768211, 1.000000000000000000, 0.9510565162951535312, 1.000000000000000000, 0.9510565162951535312, 1.000000000000000000, 0.9510565162951535312, 1.000000000000000000, 0.9510565162951535312, 1.000000000000000000, 0.9755282581475765991, 0.9755282581475768211 ) ) 
 REPRESENTATION_ITEM ( '' )  );
#21057 = CARTESIAN_POINT ( 'NONE',  ( 46.10157429594899270, 91.73445800887257917, 29.95742577749337343 ) ) ;
#21058 = CARTESIAN_POINT ( 'NONE',  ( -151.4692556286852891, -196.9891397928655010, 49.65701158161630957 ) ) ;
#21060 = CARTESIAN_POINT ( 'NONE',  ( 62.38089001705685632, 99.52138843117178624, -6.434471705120163421 ) ) ;
#21059 = CARTESIAN_POINT ( 'NONE',  ( 40.27526882409969033, 104.6651871740939868, 30.44471234641811819 ) ) ;
#21061 = CARTESIAN_POINT ( 'NONE',  ( 43.01140435219951286, 62.96049967264874425, 28.95336869806222779 ) ) ;
#21063 = CARTESIAN_POINT ( 'NONE',  ( 44.55648932407425633, 61.88445800887257064, 29.45539723777780239 ) ) ;
#21062 = CARTESIAN_POINT ( 'NONE',  ( 46.06808526308733320, 144.7210371994902403, 38.18123243450563820 ) ) ;
#21064 =( LENGTH_UNIT ( ) NAMED_UNIT ( * ) SI_UNIT ( .MILLI., .METRE. ) );
#21065 = CARTESIAN_POINT ( 'NONE',  ( 149.5529451524149920, 187.4828467975320336, 14.00000000000001776 ) ) ;
#21066 = DIRECTION ( 'NONE',  ( -1.000000000000000000, 0.000000000000000000, 0.000000000000000000 ) ) ;
#21067 = CARTESIAN_POINT ( 'NONE',  ( 47.43856463449117200, 73.46518717409398391, 35.64915139335016647 ) ) ;
#21068 = CARTESIAN_POINT ( 'NONE',  ( 64.59149290518072917, 93.33317027722591774, -7.422718449586769296 ) ) ;
#21069 = CARTESIAN_POINT ( 'NONE',  ( 43.01140435219957681, 71.03445800887256212, 29.21067981925356705 ) ) ;
#21070 = CARTESIAN_POINT ( 'NONE',  ( -151.4692556286852891, -172.1438272943107108, 59.56931450028537967 ) ) ;
#21071 = DIRECTION ( 'NONE',  ( -0.000000000000000000, 1.000000000000000000, -0.000000000000000000 ) ) ;
#21072 = ORIENTED_EDGE ( 'NONE', *, *, #20919, .F. ) ;
#21073 = CARTESIAN_POINT ( 'NONE',  ( -145.6429501568359797, -180.2084106276440707, 41.63779006702063867 ) ) ;
#21074 = CARTESIAN_POINT ( 'NONE',  ( 66.97354912532109950, 95.34500505098478129, 5.477698430975745048 ) ) ;
#21075 = ORIENTED_EDGE ( 'NONE', *, *, #4067, .F. ) ;
#21076 = CARTESIAN_POINT ( 'NONE',  ( 44.37947211624943833, 137.2151871740940123, 30.00020018409699318 ) ) ;
#21077 = CARTESIAN_POINT ( 'NONE',  ( 47.43856463449117911, 154.7651871740940237, 32.77220824515697473 ) ) ;
#21078 = CARTESIAN_POINT ( 'NONE',  ( 43.01140435219951286, 95.62977050742732388, 29.55568802177586107 ) ) ;
#21079 = EDGE_LOOP ( 'NONE', ( #15857, #4944, #12746, #14723 ) ) ;
#21080 = ORIENTED_EDGE ( 'NONE', *, *, #15000, .F. ) ;
#21081 = ADVANCED_FACE ( 'NONE', ( #17804 ), #9782, .T. ) ;
#21082 = CARTESIAN_POINT ( 'NONE',  ( 16.56453993303484395, 129.6948329502664308, 9.561135973024818213 ) ) ;
#21083 = ORIENTED_EDGE ( 'NONE', *, *, #11834, .F. ) ;
#21084 = EDGE_CURVE ( 'NONE', #14442, #18977, #10110, .T. ) ;
#21085 = CARTESIAN_POINT ( 'NONE',  ( 48.01140435219951996, 112.1344580088725706, 35.83527830041810347 ) ) ;
#21086 = CARTESIAN_POINT ( 'NONE',  ( 147.5268905834513475, 193.0332408774651185, -19.99999999999997868 ) ) ;
#21087 = CARTESIAN_POINT ( 'NONE',  ( 45.74753988029933538, 73.42977050742732104, 37.97664729208901946 ) ) ;
#21088 = CARTESIAN_POINT ( 'NONE',  ( 45.74753988029933538, 139.1651871740940010, 37.97664729208901946 ) ) ;
#21089 = CARTESIAN_POINT ( 'NONE',  ( 38.01140435219951996, 90.56049967264874567, 32.58608133808903773 ) ) ;
#21090 = CARTESIAN_POINT ( 'NONE',  ( 22.46358530849972723, 92.52609567587644790, 8.053519324161520387 ) ) ;
#21091 = CARTESIAN_POINT ( 'NONE',  ( 39.95472344131171383, 95.09311803772094152, 38.18123243450565951 ) ) ;
#21092 = CARTESIAN_POINT ( 'NONE',  ( -143.3790856849358306, -156.6891397928654612, 43.77915905869157598 ) ) ;
#21093 = CARTESIAN_POINT ( 'NONE',  ( 138.4989748031516967, 208.9305787985672680, -44.99999999999997158 ) ) ;
#21094 = CARTESIAN_POINT ( 'NONE',  ( -151.4692556286852891, -136.9891397928655010, 49.65701158161630957 ) ) ;
#21095 = CARTESIAN_POINT ( 'NONE',  ( -161.4692556286852891, -163.7130981290892748, 46.40781461928724383 ) ) ;
#21096 = EDGE_LOOP ( 'NONE', ( #17309, #1279, #4713, #21083, #2873 ) ) ;
#21097 = CARTESIAN_POINT ( 'NONE',  ( 47.43856463449117200, 79.72977050742728977, 35.64915139335016647 ) ) ;
#21098 = CARTESIAN_POINT ( 'NONE',  ( -160.8964159109769696, -164.0438272943107449, 46.59394152635518793 ) ) ;
#21099 = CARTESIAN_POINT ( 'NONE',  ( 23.17700876947760591, 147.8092992330439586, -3.851376987104358829 ) ) ;
#21100 = DIRECTION ( 'NONE',  ( -0.4999746373018760792, 0.000000000000000000, -0.8660400464498494433 ) ) ;
#21101 = ORIENTED_EDGE ( 'NONE', *, *, #3369, .F. ) ;
#21102 = DIRECTION ( 'NONE',  ( 1.000000000000000000, 0.000000000000000000, 0.000000000000000000 ) ) ;
#21103 = AXIS2_PLACEMENT_3D ( 'NONE', #19363, #13962, #19046 ) ;
#21104 = LINE ( 'NONE', #4123, #15893 ) ;
#21105 = CARTESIAN_POINT ( 'NONE',  ( 47.43856463449117911, 121.7297705074273040, 35.64915139335015937 ) ) ;
#21106 = EDGE_LOOP ( 'NONE', ( #5936, #16499, #18547, #1392 ) ) ;
#21107 = DIRECTION ( 'NONE',  ( -0.000000000000000000, -0.000000000000000000, -1.000000000000000000 ) ) ;
#21108 = ORIENTED_EDGE ( 'NONE', *, *, #10803, .T. ) ;
#21109 = CARTESIAN_POINT ( 'NONE',  ( 43.01140435219951286, 122.6297705074273239, 29.55568802177586463 ) ) ;
#21110 = CARTESIAN_POINT ( 'NONE',  ( 48.01140435219951996, 110.2104996726487514, 34.21067981925357060 ) ) ;
#21111 = CARTESIAN_POINT ( 'NONE',  ( 38.58424406990784661, 90.22977050742731819, 32.77220824515698183 ) ) ;
#21112 = CARTESIAN_POINT ( 'NONE',  ( -32.30114424549768870, -19.06233958201669410, -19.99999999999997513 ) ) ;
#21113 = CARTESIAN_POINT ( 'NONE',  ( 5.130598475945862827E-15, 0.000000000000000000, 10.00000000000001599 ) ) ;
#21114 = CARTESIAN_POINT ( 'NONE',  ( -159.5594255724347761, -188.1891397928654612, 55.53486410454104316 ) ) ;
#21115 = FACE_OUTER_BOUND ( 'NONE', #11029, .T. ) ;
#21116 = DIRECTION ( 'NONE',  ( 0.000000000000000000, -1.000000000000000000, 0.000000000000000000 ) ) ;
#21117 = CARTESIAN_POINT ( 'NONE',  ( -154.5594255724347761, -158.1630981290892919, 40.14644641866476604 ) ) ;
#21118 = SHAPE_DEFINITION_REPRESENTATION ( #12013, #8609 ) ;
#21119 = CARTESIAN_POINT ( 'NONE',  ( 48.01140435219951996, 136.1344580088725991, 35.83527830041810347 ) ) ;
#21120 = CARTESIAN_POINT ( 'NONE',  ( 38.58424406990784661, 102.5297705074273154, 35.64915139335016647 ) ) ;
#21121 = CARTESIAN_POINT ( 'NONE',  ( 22.18708823908250238, 100.7722391081675255, 7.342430719951936524 ) ) ;
#21122 = CARTESIAN_POINT ( 'NONE',  ( 125.6223472235027998, 193.0332408774651185, 14.00000000000001776 ) ) ;
#21123 = CARTESIAN_POINT ( 'NONE',  ( 45.74753988029934249, 100.1651871740939868, 37.97664729208901235 ) ) ;
#21124 = CARTESIAN_POINT ( 'NONE',  ( -151.4692556286853176, -162.8130981290893260, 59.65701158161632378 ) ) ;
#21125 = ORIENTED_EDGE ( 'NONE', *, *, #13071, .T. ) ;
#21126 = EDGE_CURVE ( 'NONE', #12769, #9727, #15280, .T. ) ;
#21127 = CARTESIAN_POINT ( 'NONE',  ( 46.10157429594899270, 157.7344580088725934, 29.95742577749336988 ) ) ;
#21128 = CARTESIAN_POINT ( 'NONE',  ( 46.60148787037231699, 85.86292235506145687, 7.220022382731924537 ) ) ;
#21129 = CARTESIAN_POINT ( 'NONE',  ( 29.44877014884911404, 144.5398477306827942, -9.648498702473171207 ) ) ;
#21130 = CARTESIAN_POINT ( 'NONE',  ( 46.10157429594899270, 153.8344580088725877, 38.46393386101375711 ) ) ;
#21131 = CARTESIAN_POINT ( 'NONE',  ( 47.43856463449117911, 74.02977050742730114, 32.77220824515697473 ) ) ;
#21132 = ORIENTED_EDGE ( 'NONE', *, *, #17075, .T. ) ;
#21133 = ORIENTED_EDGE ( 'NONE', *, *, #7576, .T. ) ;
#21134 = CARTESIAN_POINT ( 'NONE',  ( 38.58424406990784661, 153.2297705074273608, 32.77220824515698183 ) ) ;
#21135 = CARTESIAN_POINT ( 'NONE',  ( 125.6223472235027998, 193.0332408774651185, 14.00000000000001776 ) ) ;
#21136 = CARTESIAN_POINT ( 'NONE',  ( 48.01140435219951996, 122.0604996726487315, 35.83527830041810347 ) ) ;
#21138 = CARTESIAN_POINT ( 'NONE',  ( 13.96574040630659752, 137.8735611475157157, -3.299202782472894224 ) ) ;
#21137 = CARTESIAN_POINT ( 'NONE',  ( 47.43856463449117200, 79.46518717409399812, 35.64915139335016647 ) ) ;
#21139 = CARTESIAN_POINT ( 'NONE',  ( -151.4692556286852891, -173.6438272943107108, 39.74470866294723947 ) ) ;
#21140 = CARTESIAN_POINT ( 'NONE',  ( 30.18028515090310293, 151.2280014487710957, 17.43780275515693390 ) ) ;
#21141 = CARTESIAN_POINT ( 'NONE',  ( -143.3790856849358306, -192.3630981290893089, 55.53486410454105027 ) ) ;
#21142 = LINE ( 'NONE', #6027, #6505 ) ;
#21143 = CARTESIAN_POINT ( 'NONE',  ( -148.3790856849358306, -162.3891397928654499, 40.14644641866477315 ) ) ;
#21144 = CARTESIAN_POINT ( 'NONE',  ( 47.43856463449118621, 130.8797705074273381, 34.21067981925357060 ) ) ;
#21145 = CARTESIAN_POINT ( 'NONE',  ( 20.86407471411557779, 93.69780688484533471, 0.1205864258981524662 ) ) ;
#21146 = CARTESIAN_POINT ( 'NONE',  ( 47.43856463449117911, 124.4651871740940123, 35.64915139335015937 ) ) ;
#21147 = EDGE_CURVE ( 'NONE', #488, #13376, #19329, .T. ) ;
#21148 = CARTESIAN_POINT ( 'NONE',  ( 43.01140435219951286, 137.9604996726487514, 29.21067981925356705 ) ) ;
#21149 = CARTESIAN_POINT ( 'NONE',  ( -154.3824083646099439, -158.7584106276440536, 40.69124936498395328 ) ) ;
#21150 = DIRECTION ( 'NONE',  ( -1.186952418100008983E-16, -0.000000000000000000, -1.000000000000000000 ) ) ;
#21151 = CARTESIAN_POINT ( 'NONE',  ( -154.5594255724347761, -156.0891397928654953, 40.14644641866476604 ) ) ;
#21152 = CARTESIAN_POINT ( 'NONE',  ( 35.68099593698222094, 147.2217917141817907, 16.62841781073025871 ) ) ;
#21153 = CARTESIAN_POINT ( 'NONE',  ( 46.10157429594899270, 83.66049967264873999, 29.95742577749336988 ) ) ;
#21154 = CARTESIAN_POINT ( 'NONE',  ( 38.58424406990784661, 108.2651871740939953, 35.64915139335016647 ) ) ;
#21155 = EDGE_LOOP ( 'NONE', ( #445, #19517, #14896, #3540 ) ) ;
#21156 = CARTESIAN_POINT ( 'NONE',  ( -151.4692556286852891, -196.9891397928655010, 59.65701158161632378 ) ) ;
#21157 = ORIENTED_EDGE ( 'NONE', *, *, #18788, .T. ) ;
#21158 = CARTESIAN_POINT ( 'NONE',  ( 47.05648932407426344, 90.98445800887257917, 37.14960608071593384 ) ) ;
#21159 = DIRECTION ( 'NONE',  ( 0.000000000000000000, 0.000000000000000000, -1.000000000000000000 ) ) ;
#21160 = CARTESIAN_POINT ( 'NONE',  ( 46.10157429594899270, 151.7604996726487059, 38.46393386101376421 ) ) ;
#21162 = CARTESIAN_POINT ( 'NONE',  ( 55.45346087869361185, 145.1240540049360845, -8.577242388453932165 ) ) ;
#21161 = CARTESIAN_POINT ( 'NONE',  ( 45.74753988029933538, 106.1651871740940152, 37.97664729208901946 ) ) ;
#21163 = CARTESIAN_POINT ( 'NONE',  ( 41.46631938032478359, 63.11049967264874283, 29.45539723777780239 ) ) ;
#21165 = CARTESIAN_POINT ( 'NONE',  ( 43.01140435219951996, 10.71049967264875491, 34.21067981925357060 ) ) ;
#21164 = CARTESIAN_POINT ( 'NONE',  ( 47.35193302267275328, 144.5280796467438620, 36.71405245301005493 ) ) ;
#21166 = CARTESIAN_POINT ( 'NONE',  ( 48.01140435219951996, 79.28445800887259054, 34.21067981925357060 ) ) ;
#21167 = DIRECTION ( 'NONE',  ( 1.915514545828640458E-16, 7.041092946335503408E-17, 1.000000000000000000 ) ) ;
#21168 = CARTESIAN_POINT ( 'NONE',  ( 43.01140435219951286, 71.36518717409397539, 29.55568802177586463 ) ) ;
#21169 = CARTESIAN_POINT ( 'NONE',  ( 47.47886434171987702, 153.8471147930492862, -3.017879606865911502 ) ) ;
#21170 = CARTESIAN_POINT ( 'NONE',  ( 39.92123440845005433, 114.2604996726487343, 29.95742577749336988 ) ) ;
#21171 = CARTESIAN_POINT ( 'NONE',  ( -160.8964159109769696, -166.7438272943107336, 52.72008163687743121 ) ) ;
#21172 = CARTESIAN_POINT ( 'NONE',  ( -145.6429501568359797, -186.2084106276440423, 41.63779006702063867 ) ) ;
#21173 = ORIENTED_EDGE ( 'NONE', *, *, #6919, .T. ) ;
#21174 = CARTESIAN_POINT ( 'NONE',  ( -160.8964159109769696, -170.0084106276440252, 52.72008163687743121 ) ) ;
#21175 = CARTESIAN_POINT ( 'NONE',  ( 63.63589212299756070, 92.48244826560708987, 12.62055557379543203 ) ) ;
#21176 = EDGE_LOOP ( 'NONE', ( #18192, #9971, #18960, #10131, #11800, #17637 ) ) ;
#21177 = CARTESIAN_POINT ( 'NONE',  ( 41.64333658814960870, 137.5151871740939953, 30.00020018409699318 ) ) ;
#21178 = CARTESIAN_POINT ( 'NONE',  ( 41.64333658814960870, 156.7151871740939839, 38.42115945441014446 ) ) ;
#21179 =( BOUNDED_CURVE ( )  B_SPLINE_CURVE ( 2, ( #6129, #19697, #16271, #3162, #1288, #14728, #12859, #19580, #18140, #6242, #14615, #21353, #21464 ),
 .UNSPECIFIED., .F., .F. ) 
 B_SPLINE_CURVE_WITH_KNOTS ( ( 3, 2, 2, 2, 2, 2, 3 ),
 ( 0.9044117647058823595, 0.9058823529411764719, 0.9088235294117646967, 0.9117647058823529216, 0.9147058823529411464, 0.9176470588235293713, 0.9191176470588234837 ),
 .UNSPECIFIED. ) 
 CURVE ( )  GEOMETRIC_REPRESENTATION_ITEM ( )  RATIONAL_B_SPLINE_CURVE ( ( 0.9755282581475768211, 0.9755282581475768211, 1.000000000000000000, 0.9510565162951535312, 1.000000000000000000, 0.9510565162951535312, 1.000000000000000000, 0.9510565162951535312, 1.000000000000000000, 0.9510565162951535312, 1.000000000000000000, 0.9755282581475768211, 0.9755282581475768211 ) ) 
 REPRESENTATION_ITEM ( '' )  );
#21180 = CARTESIAN_POINT ( 'NONE',  ( 45.74753988029934249, 92.32977050742731251, 30.44471234641812174 ) ) ;
#21181 = ORIENTED_EDGE ( 'NONE', *, *, #3207, .T. ) ;
#21182 = ORIENTED_EDGE ( 'NONE', *, *, #18533, .T. ) ;
#21183 = AXIS2_PLACEMENT_3D ( 'NONE', #8194, #9630, #13254 ) ;
#21184 = CIRCLE ( 'NONE', #11669, 3.000000000000050626 ) ;
#21185 = CARTESIAN_POINT ( 'NONE',  ( 32.23767430054768823, 145.5917660130458842, 17.43780275515694456 ) ) ;
#21186 = ORIENTED_EDGE ( 'NONE', *, *, #15515, .F. ) ;
#21187 = PRODUCT_DEFINITION ( 'UNKNOWN', '', #21476, #15236 ) ;
#21188 = CARTESIAN_POINT ( 'NONE',  ( 53.01140435219953417, 119.9070776186055838, -35.00000000000000000 ) ) ;
#21189 = AXIS2_PLACEMENT_3D ( 'NONE', #1839, #13619, #10003 ) ;
#21190 = CARTESIAN_POINT ( 'NONE',  ( 44.37947211624943833, 73.27977050742731535, 38.42115945441014446 ) ) ;
#21191 = CARTESIAN_POINT ( 'NONE',  ( 45.74753988029933538, 131.0651871740940067, 30.44471234641811819 ) ) ;
#21192 = CARTESIAN_POINT ( 'NONE',  ( 39.92123440845004723, 88.16049967264873999, 38.46393386101376421 ) ) ;
#21193 = CARTESIAN_POINT ( 'NONE',  ( 53.04203944364535772, 87.17698241397053494, 14.00585298808814194 ) ) ;
#21194 = EDGE_CURVE ( 'NONE', #470, #14339, #21371, .T. ) ;
#21195 = CARTESIAN_POINT ( 'NONE',  ( 38.17234397690566539, 95.37979192033441223, 32.91075569967800618 ) ) ;
#21196 = CARTESIAN_POINT ( 'NONE',  ( -154.5594255724347761, -162.0891397928654669, 40.14644641866476604 ) ) ;
#21197 = LINE ( 'NONE', #6083, #612 ) ;
#21198 = VECTOR ( 'NONE', #7009, 1000.000000000000000 ) ;
#21199 = LINE ( 'NONE', #1461, #13440 ) ;
#21200 = AXIS2_PLACEMENT_3D ( 'NONE', #6788, #5119, #13703 ) ;
#21201 = ORIENTED_EDGE ( 'NONE', *, *, #17267, .F. ) ;
#21202 = CARTESIAN_POINT ( 'NONE',  ( 38.58424406990784661, 72.52977050742731535, 35.64915139335016647 ) ) ;
#21203 = CARTESIAN_POINT ( 'NONE',  ( -157.2955611005346270, -194.6084106276440195, 41.63779006702063867 ) ) ;
#21204 = ADVANCED_FACE ( 'NONE', ( #1728 ), #1835, .T. ) ;
#21205 = CARTESIAN_POINT ( 'NONE',  ( 66.89036333300305159, 144.4373801540182569, -2.303882249869787291 ) ) ;
#21206 = PLANE ( 'NONE',  #15720 ) ;
#21207 = AXIS2_PLACEMENT_3D ( 'NONE', #19780, #3023, #21222 ) ;
#21208 = VERTEX_POINT ( 'NONE', #13300 ) ;
#21209 = CARTESIAN_POINT ( 'NONE',  ( -161.4692556286852891, -161.3391397928654669, 52.90620854394536821 ) ) ;
#21210 = CARTESIAN_POINT ( 'NONE',  ( 38.96631938032478359, 104.4844580088725650, 31.27175355779120025 ) ) ;
#21211 = CARTESIAN_POINT ( 'NONE',  ( 44.37947211624943833, 124.2797705074273154, 38.42115945441014446 ) ) ;
#21212 = EDGE_CURVE ( 'NONE', #17591, #9530, #1806, .T. ) ;
#21213 = VERTEX_POINT ( 'NONE', #8671 ) ;
#21214 = CARTESIAN_POINT ( 'NONE',  ( 43.01140435219954838, 131.0344580088725479, 29.21067981925356705 ) ) ;
#21215 = ORIENTED_EDGE ( 'NONE', *, *, #6493, .T. ) ;
#21216 = CARTESIAN_POINT ( 'NONE',  ( 47.43856463449117200, 130.7297705074273040, 35.64915139335016647 ) ) ;
#21217 = DIRECTION ( 'NONE',  ( -0.000000000000000000, 1.000000000000000000, -0.000000000000000000 ) ) ;
#21218 = CARTESIAN_POINT ( 'NONE',  ( 41.64333658814960870, 89.77977050742731535, 30.00020018409699318 ) ) ;
#21219 = CARTESIAN_POINT ( 'NONE',  ( 39.92123440845004723, 59.33445800887256638, 29.95742577749337343 ) ) ;
#21220 = EDGE_CURVE ( 'NONE', #8083, #14631, #8462, .T. ) ;
#21221 = DIRECTION ( 'NONE',  ( -0.000000000000000000, -0.000000000000000000, -1.000000000000000000 ) ) ;
#21222 = DIRECTION ( 'NONE',  ( -0.3428981916074324565, 0.9393725726208703719, 0.000000000000000000 ) ) ;
#21223 = CARTESIAN_POINT ( 'NONE',  ( 43.01140435219951286, 95.96049967264873715, 29.21067981925356705 ) ) ;
#21224 = CARTESIAN_POINT ( 'NONE',  ( -161.4692556286853176, -185.4891397928654726, 49.65701158161630957 ) ) ;
#21225 = CARTESIAN_POINT ( 'NONE',  ( 46.10157429594899270, 133.7344580088725650, 29.95742577749336988 ) ) ;
#21226 = CARTESIAN_POINT ( 'NONE',  ( -38.21168032741934439, -23.19216891395253910, 4.000000000000021316 ) ) ;
#21227 = CARTESIAN_POINT ( 'NONE',  ( -160.8964159109769696, -187.8938272943107393, 49.65701158161630957 ) ) ;
#21228 = SHAPE_DEFINITION_REPRESENTATION ( #13775, #6933 ) ;
#21229 = ADVANCED_FACE ( 'NONE', ( #9889, #3495 ), #16588, .T. ) ;
#21230 = CARTESIAN_POINT ( 'NONE',  ( 44.55648932407425633, 123.6844580088725820, 38.96596240072933170 ) ) ;
#21231 = CARTESIAN_POINT ( 'NONE',  ( 47.43856463449117200, 101.0297705074273011, 32.77220824515698183 ) ) ;
#21232 = CARTESIAN_POINT ( 'NONE',  ( 37.76446383830448639, 92.11682557054228937, 6.628417810721723313 ) ) ;
#21233 = CARTESIAN_POINT ( 'NONE',  ( -160.8964159109769696, -194.0438272943107165, 46.59394152635518793 ) ) ;
#21234 = CARTESIAN_POINT ( 'NONE',  ( 44.37947211624943833, 100.0151871740939953, 38.42115945441014446 ) ) ;
#21235 = DIRECTION ( 'NONE',  ( 0.000000000000000000, -1.000000000000000000, 0.000000000000000000 ) ) ;
#21236 = VERTEX_POINT ( 'NONE', #11745 ) ;
#21237 = DIRECTION ( 'NONE',  ( -0.5010362705417047424, 0.000000000000000000, -0.8654262854811261008 ) ) ;
#21238 = CARTESIAN_POINT ( 'NONE',  ( 20.22230697948889500, 94.36241449208007737, 1.148710122009321211 ) ) ;
#21239 = CARTESIAN_POINT ( 'NONE',  ( 43.01140435219951286, 145.1297705074273097, 38.86567161673127657 ) ) ;
#21240 = CARTESIAN_POINT ( 'NONE',  ( 20.72232308940363765, 137.1362251821529696, 16.90007324815861267 ) ) ;
#21241 = CARTESIAN_POINT ( 'NONE',  ( 47.47886434171987702, 153.8471147930492862, -3.017879606865911502 ) ) ;
#21242 = CARTESIAN_POINT ( 'NONE',  ( 38.58424406990786082, 66.37977050742730967, 34.21067981925357060 ) ) ;
#21243 = ORIENTED_EDGE ( 'NONE', *, *, #12549, .F. ) ;
#21244 = ORIENTED_EDGE ( 'NONE', *, *, #13822, .F. ) ;
#21245 = CARTESIAN_POINT ( 'NONE',  ( 38.58424406990786082, 153.3797705074273097, 34.21067981925357060 ) ) ;
#21246 =( BOUNDED_CURVE ( )  B_SPLINE_CURVE ( 2, ( #21499, #19837, #3080, #18174, #21610, #16513, #3305, #5068, #2968, #9707, #1318, #9924, #13115 ),
 .UNSPECIFIED., .F., .F. ) 
 B_SPLINE_CURVE_WITH_KNOTS ( ( 3, 2, 2, 2, 2, 2, 3 ),
 ( 0.4821428571428571508, 0.4857142857142857095, 0.4928571428571428825, 0.5000000000000000000, 0.5071428571428571175, 0.5142857142857142350, 0.5178571428571429047 ),
 .UNSPECIFIED. ) 
 CURVE ( )  GEOMETRIC_REPRESENTATION_ITEM ( )  RATIONAL_B_SPLINE_CURVE ( ( 0.9755282581475768211, 0.9755282581475768211, 1.000000000000000000, 0.9510565162951535312, 1.000000000000000000, 0.9510565162951535312, 1.000000000000000000, 0.9510565162951535312, 1.000000000000000000, 0.9510565162951535312, 1.000000000000000000, 0.9755282581475763770, 0.9755282581475768211 ) ) 
 REPRESENTATION_ITEM ( '' )  );
#21247 = CARTESIAN_POINT ( 'NONE',  ( -154.5594255724347761, -194.1630981290892919, 40.14644641866476604 ) ) ;
#21248 = CARTESIAN_POINT ( 'NONE',  ( 39.92123440845004723, 120.2604996726487485, 29.95742577749337343 ) ) ;
#21250 = CARTESIAN_POINT ( 'NONE',  ( 75.45202302719175691, 109.2280190411066059, 6.938704244663667531 ) ) ;
#21249 = CARTESIAN_POINT ( 'NONE',  ( 44.37947211624943833, 70.01518717409399528, 38.42115945441014446 ) ) ;
#21251 = CARTESIAN_POINT ( 'NONE',  ( -160.8964159109769696, -175.8938272943107393, 49.65701158161630957 ) ) ;
#21252 = CARTESIAN_POINT ( 'NONE',  ( 70.62757080055673953, 99.67629488849819097, 13.29148015538516425 ) ) ;
#21253 = CARTESIAN_POINT ( 'NONE',  ( -161.4692556286852607, -178.7130981290893317, 46.40781461928724383 ) ) ;
#21254 = FACE_OUTER_BOUND ( 'NONE', #9944, .T. ) ;
#21255 = CARTESIAN_POINT ( 'NONE',  ( 147.8787791192428074, -126.9891397928655010, -9.657011581616311346 ) ) ;
#21256 = CARTESIAN_POINT ( 'NONE',  ( 38.58424406990784661, 135.2297705074273324, 32.77220824515698183 ) ) ;
#21257 = CARTESIAN_POINT ( 'NONE',  ( 58.01262221917386341, 89.04620360302797621, 5.834872140203966495 ) ) ;
#21258 = CARTESIAN_POINT ( 'NONE',  ( 47.43856463449117911, 130.4651871740939839, 35.64915139335015937 ) ) ;
#21259 = FACE_OUTER_BOUND ( 'NONE', #369, .T. ) ;
#21260 = DIRECTION ( 'NONE',  ( 1.000000000000000000, 0.000000000000000000, -0.000000000000000000 ) ) ;
#21261 = DIRECTION ( 'NONE',  ( 1.000000000000000000, 0.000000000000000000, -0.000000000000000000 ) ) ;
#21262 = FACE_OUTER_BOUND ( 'NONE', #19681, .T. ) ;
#21263 = CARTESIAN_POINT ( 'NONE',  ( 71.13433436327568415, 121.9840874124550965, -8.414894741535439593 ) ) ;
#21264 = CARTESIAN_POINT ( 'NONE',  ( 173.3794444120442506, -126.9891397928655010, 67.64809332337412684 ) ) ;
#21265 = CARTESIAN_POINT ( 'NONE',  ( 41.64333658814960870, 108.7151871740940123, 38.42115945441014446 ) ) ;
#21266 = ORIENTED_EDGE ( 'NONE', *, *, #4921, .F. ) ;
#21267 = CARTESIAN_POINT ( 'NONE',  ( -23.27144139456156324, -18.88988604584387332, 4.000000000000021316 ) ) ;
#21268 = ORIENTED_EDGE ( 'NONE', *, *, #14584, .T. ) ;
#21269 = CARTESIAN_POINT ( 'NONE',  ( 46.10157429594899270, 81.83445800887258770, 38.46393386101376421 ) ) ;
#21270 = CARTESIAN_POINT ( 'NONE',  ( -91.10645082872859746, 10.96617311717548660, 4.000000000000021316 ) ) ;
#21271 = ADVANCED_FACE ( 'NONE', ( #1507 ), #1612, .F. ) ;
#21272 = CARTESIAN_POINT ( 'NONE',  ( 39.92123440845004723, 150.2604996726487911, 29.95742577749337343 ) ) ;
#21274 = CARTESIAN_POINT ( 'NONE',  ( 16.30727314429931241, 128.7156746967485788, -10.48204345529337189 ) ) ;
#21273 = CARTESIAN_POINT ( 'NONE',  ( 40.27526882409969033, 108.5651871740939924, 37.97664729208901946 ) ) ;
#21275 = CARTESIAN_POINT ( 'NONE',  ( 48.01140435219951996, 65.36049967264874283, 32.58608133808903773 ) ) ;
#21277 = CARTESIAN_POINT ( 'NONE',  ( -151.4692556286852891, -182.3130981290892976, 39.65701158161629536 ) ) ;
#21276 = CARTESIAN_POINT ( 'NONE',  ( 47.97935898834261081, 144.4085802287884803, 34.86345644064633831 ) ) ;
#21278 = CARTESIAN_POINT ( 'NONE',  ( 47.05648932407426344, 117.9844580088725792, 37.14960608071593384 ) ) ;
#21279 = CARTESIAN_POINT ( 'NONE',  ( 48.01140435219951996, 79.13445800887257064, 35.83527830041809636 ) ) ;
#21280 = DIRECTION ( 'NONE',  ( 1.000000000000000000, 0.000000000000000000, 0.000000000000000000 ) ) ;
#21281 = CARTESIAN_POINT ( 'NONE',  ( 40.27526882409969033, 62.66518717409400097, 30.44471234641811819 ) ) ;
#21282 = CARTESIAN_POINT ( 'NONE',  ( 71.86557814238962294, 101.4853659568252766, -7.779689512009451136 ) ) ;
#21283 = AXIS2_PLACEMENT_3D ( 'NONE', #12151, #14024, #20758 ) ;
#21284 = EDGE_CURVE ( 'NONE', #11408, #17105, #4050, .T. ) ;
#21285 = CARTESIAN_POINT ( 'NONE',  ( 39.92123440845005433, 115.1604996726487400, 38.46393386101375711 ) ) ;
#21286 = CARTESIAN_POINT ( 'NONE',  ( -160.8964159109769696, -175.8938272943107393, 49.65701158161630957 ) ) ;
#21287 = CARTESIAN_POINT ( 'NONE',  ( -142.0420953463935803, -183.5084106276440252, 46.59394152635518083 ) ) ;
#21288 = ORIENTED_EDGE ( 'NONE', *, *, #17549, .F. ) ;
#21289 = MECHANICAL_DESIGN_GEOMETRIC_PRESENTATION_REPRESENTATION (  '', ( #8969 ), #14280 ) ;
#21290 = CARTESIAN_POINT ( 'NONE',  ( 43.01140435219951286, 65.36518717409398960, 29.55568802177586107 ) ) ;
#21291 = CARTESIAN_POINT ( 'NONE',  ( -159.0959885057557983, -166.8584106276440480, 55.19815736654470584 ) ) ;
#21292 = CARTESIAN_POINT ( 'NONE',  ( 66.46241511549931147, 94.85692098654722315, 12.50163586956050210 ) ) ;
#21293 =( NAMED_UNIT ( * ) SI_UNIT ( $, .STERADIAN. ) SOLID_ANGLE_UNIT ( ) );
#21294 = CARTESIAN_POINT ( 'NONE',  ( 47.43856463449117200, 136.4651871740939839, 35.64915139335016647 ) ) ;
#21295 = VERTEX_POINT ( 'NONE', #20461 ) ;
#21296 = ORIENTED_EDGE ( 'NONE', *, *, #13990, .T. ) ;
#21297 = EDGE_LOOP ( 'NONE', ( #7582, #16362, #337, #2150 ) ) ;
#21298 = CARTESIAN_POINT ( 'NONE',  ( 46.10157429594899270, 115.7344580088725650, 29.95742577749337343 ) ) ;
#21299 = CARTESIAN_POINT ( 'NONE',  ( 45.51148226160370314, 59.71123016864974176, 29.88059778228138086 ) ) ;
#21300 = CARTESIAN_POINT ( 'NONE',  ( 40.27526882409969033, 78.82977050742731251, 37.97664729208901946 ) ) ;
#21301 = CARTESIAN_POINT ( 'NONE',  ( 47.43856463449117200, 136.7651871740939953, 32.77220824515698183 ) ) ;
#21302 = CARTESIAN_POINT ( 'NONE',  ( 46.10157429594899270, 92.66049967264873999, 29.95742577749337343 ) ) ;
#21303 = CARTESIAN_POINT ( 'NONE',  ( 17.14282613681034917, 97.48634091255654255, 8.291567264837656381 ) ) ;
#21304 = CARTESIAN_POINT ( 'NONE',  ( 43.01140435219951996, 94.90707761860558378, 29.21067981925357060 ) ) ;
#21305 = CARTESIAN_POINT ( 'NONE',  ( -141.4692556286852891, -162.8391397928654101, 46.40781461928724383 ) ) ;
#21306 = ADVANCED_FACE ( 'NONE', ( #3704 ), #12507, .F. ) ;
#21307 = LINE ( 'NONE', #14787, #7319 ) ;
#21308 = CARTESIAN_POINT ( 'NONE',  ( 47.05648932407426344, 62.51049967264874141, 31.27175355779120025 ) ) ;
#21309 = ORIENTED_EDGE ( 'NONE', *, *, #12044, .F. ) ;
#21310 = CARTESIAN_POINT ( 'NONE',  ( 47.43856463449117200, 70.72977050742730398, 35.64915139335016647 ) ) ;
#21311 = CARTESIAN_POINT ( 'NONE',  ( -145.6429501568359797, -158.9438272943107222, 41.63779006702063867 ) ) ;
#21312 = CARTESIAN_POINT ( 'NONE',  ( 72.98789752971651978, 103.3738663174133023, 6.148623012889737005 ) ) ;
#21313 = CARTESIAN_POINT ( 'NONE',  ( -151.4692556286852891, -185.9084106276440025, 39.74470866294723947 ) ) ;
#21314 = VERTEX_POINT ( 'NONE', #8994 ) ;
#21315 = LINE ( 'NONE', #11269, #13243 ) ;
#21316 = EDGE_CURVE ( 'NONE', #19655, #19660, #4132, .T. ) ;
#21317 = CARTESIAN_POINT ( 'NONE',  ( 46.10157429594899270, 123.8344580088725735, 38.46393386101375711 ) ) ;
#21318 = CARTESIAN_POINT ( 'NONE',  ( 40.27526882409969744, 119.9297705074272926, 30.44471234641812174 ) ) ;
#21319 = ORIENTED_EDGE ( 'NONE', *, *, #20799, .F. ) ;
#21320 = AXIS2_PLACEMENT_3D ( 'NONE', #17919, #7914, #2828 ) ;
#21321 = CARTESIAN_POINT ( 'NONE',  ( 43.01140435219951996, 2.710499672648754466, 34.21067981925357060 ) ) ;
#21322 = EDGE_CURVE ( 'NONE', #17969, #4022, #10689, .T. ) ;
#21323 = ORIENTED_EDGE ( 'NONE', *, *, #4173, .T. ) ;
#21324 = CARTESIAN_POINT ( 'NONE',  ( 41.64333658814960870, 125.7797705074273296, 30.00020018409699318 ) ) ;
#21325 = CARTESIAN_POINT ( 'NONE',  ( -151.4692556286852891, -196.9891397928655010, 49.65701158161630957 ) ) ;
#21326 = CARTESIAN_POINT ( 'NONE',  ( 47.05648932407426344, 66.98445800887257917, 37.14960608071593384 ) ) ;
#21327 = EDGE_CURVE ( 'NONE', #7201, #9959, #17556, .T. ) ;
#21328 = LINE ( 'NONE', #13162, #14314 ) ;
#21329 = CARTESIAN_POINT ( 'NONE',  ( 42.21948215057684450, 102.4575765865523209, 39.21067981925355639 ) ) ;
#21330 = CARTESIAN_POINT ( 'NONE',  ( -153.0531000319306827, -175.8160212151857422, 59.65701158161631668 ) ) ;
#21331 = CARTESIAN_POINT ( 'NONE',  ( -151.4692556286852891, -187.7391397928654726, 60.17163382399899518 ) ) ;
#21332 = CARTESIAN_POINT ( 'NONE',  ( 138.2733499813809885, 177.2661675079481540, -44.99999999999997158 ) ) ;
#21333 = CARTESIAN_POINT ( 'NONE',  ( -145.6429501568359797, -186.8438272943106995, 57.67623309621198047 ) ) ;
#21334 = CARTESIAN_POINT ( 'NONE',  ( 44.55648932407425633, 127.8844580088725706, 29.45539723777780239 ) ) ;
#21335 = CARTESIAN_POINT ( 'NONE',  ( 43.01140435219951286, 100.1297705074273239, 38.86567161673127657 ) ) ;
#21336 = CARTESIAN_POINT ( 'NONE',  ( 49.02192908010439254, 147.4586317741252799, -9.843465619175002956 ) ) ;
#21337 = CARTESIAN_POINT ( 'NONE',  ( -160.8964159109769696, -184.7438272943107052, 52.72008163687743121 ) ) ;
#21338 = CARTESIAN_POINT ( 'NONE',  ( 43.01140435219951286, 95.36518717409400381, 29.55568802177586107 ) ) ;
#21339 = CARTESIAN_POINT ( 'NONE',  ( 42.21948215057684450, 85.38361825032846752, 39.21067981925355639 ) ) ;
#21340 = ORIENTED_EDGE ( 'NONE', *, *, #7813, .F. ) ;
#21341 = CYLINDRICAL_SURFACE ( 'NONE', #2038, 4.999999999999997335 ) ;
#21342 = CARTESIAN_POINT ( 'NONE',  ( 36.38086904327614235, 86.32171732562966326, 0.5532606071062302622 ) ) ;
#21343 = CARTESIAN_POINT ( 'NONE',  ( 43.27907770151751521, 148.0257240122537610, -16.07737750751418915 ) ) ;
#21344 = CARTESIAN_POINT ( 'NONE',  ( 43.01140435219951286, 67.12977050742730967, 38.86567161673127657 ) ) ;
#21345 = ORIENTED_EDGE ( 'NONE', *, *, #712, .F. ) ;
#21346 = EDGE_LOOP ( 'NONE', ( #15330, #18106, #10191, #65 ) ) ;
#21347 = CARTESIAN_POINT ( 'NONE',  ( 39.42975644700377558, 156.6797705074273210, 36.81289934271958941 ) ) ;
#21348 = VECTOR ( 'NONE', #1909, 1000.000000000000000 ) ;
#21350 = EDGE_CURVE ( 'NONE', #3570, #951, #16507, .T. ) ;
#21349 = DIRECTION ( 'NONE',  ( 0.000000000000000000, 0.000000000000000000, 1.000000000000000000 ) ) ;
#21351 = CARTESIAN_POINT ( 'NONE',  ( 41.46631938032478359, 108.1104996726487428, 29.45539723777780239 ) ) ;
#21352 = CARTESIAN_POINT ( 'NONE',  ( 41.64333658814960870, 65.51518717409400949, 30.00020018409699318 ) ) ;
#21353 = CARTESIAN_POINT ( 'NONE',  ( 42.21948215057684450, 65.11133943119283174, 29.21067981925356705 ) ) ;
#21354 = CARTESIAN_POINT ( 'NONE',  ( -145.6429501568359797, -171.8438272943107279, 57.67623309621197336 ) ) ;
#21355 = CARTESIAN_POINT ( 'NONE',  ( 163.4517194221884040, 198.8869265230379995, -19.99999999999997868 ) ) ;
#21356 = CARTESIAN_POINT ( 'NONE',  ( -141.4692556286852891, -182.9130981290893203, 46.40781461928724383 ) ) ;
#21357 = CARTESIAN_POINT ( 'NONE',  ( 44.55648932407425633, 153.6844580088725820, 38.96596240072933170 ) ) ;
#21358 = CARTESIAN_POINT ( 'NONE',  ( 43.01140435219951286, 130.1297705074273381, 38.86567161673127657 ) ) ;
#21359 = CARTESIAN_POINT ( 'NONE',  ( 25.66908397218059790, 90.29788686741908066, 13.93020729814628744 ) ) ;
#21360 = CIRCLE ( 'NONE', #4110, 15.56217413224114310 ) ;
#21361 = CARTESIAN_POINT ( 'NONE',  ( 47.43856463449117911, 127.4651871740939839, 35.64915139335015937 ) ) ;
#21362 = CARTESIAN_POINT ( 'NONE',  ( 43.01140435219951286, 92.03445800887257633, 29.21067981925356705 ) ) ;
#21363 = CARTESIAN_POINT ( 'NONE',  ( -157.2955611005345986, -157.7084106276440423, 57.67623309621197336 ) ) ;
#21364 = CARTESIAN_POINT ( 'NONE',  ( 43.01140435219951286, 65.96049967264873715, 29.21067981925356705 ) ) ;
#21365 = VECTOR ( 'NONE', #13047, 1000.000000000000000 ) ;
#21366 = CARTESIAN_POINT ( 'NONE',  ( 42.21948215057684450, 135.0373810949689926, 29.21067981925356705 ) ) ;
#21367 = CARTESIAN_POINT ( 'NONE',  ( 60.80507725967250821, 98.03074643439879310, -7.343579217248467295 ) ) ;
#21368 = CARTESIAN_POINT ( 'NONE',  ( 147.8787791192428074, -136.9891397928655010, 0.3429884183836981459 ) ) ;
#21369 = EDGE_CURVE ( 'NONE', #6932, #811, #6494, .T. ) ;
#21370 = EDGE_CURVE ( 'NONE', #17801, #12681, #13728, .T. ) ;
#21371 =( BOUNDED_CURVE ( )  B_SPLINE_CURVE ( 2, ( #11968, #10107, #18256, #18590, #1939, #16814, #20355, #3601, #6808, #290, #11526, #6911, #5036 ),
 .UNSPECIFIED., .F., .F. ) 
 B_SPLINE_CURVE_WITH_KNOTS ( ( 3, 2, 2, 2, 2, 2, 3 ),
 ( 0.1691176470588235115, 0.1705882352941176516, 0.1735294117647058765, 0.1764705882352941291, 0.1794117647058823539, 0.1823529411764705788, 0.1838235294117647189 ),
 .UNSPECIFIED. ) 
 CURVE ( )  GEOMETRIC_REPRESENTATION_ITEM ( )  RATIONAL_B_SPLINE_CURVE ( ( 0.9755282581475765991, 0.9755282581475764880, 1.000000000000000000, 0.9510565162951535312, 1.000000000000000000, 0.9510565162951535312, 1.000000000000000000, 0.9510565162951535312, 1.000000000000000000, 0.9510565162951535312, 1.000000000000000000, 0.9755282581475765991, 0.9755282581475768211 ) ) 
 REPRESENTATION_ITEM ( '' )  );
#21372 = ORIENTED_EDGE ( 'NONE', *, *, #3855, .T. ) ;
#21373 = CARTESIAN_POINT ( 'NONE',  ( 43.80332655382220253, 85.53738109496900677, 39.21067981925355639 ) ) ;
#21374 = ORIENTED_EDGE ( 'NONE', *, *, #14318, .T. ) ;
#21375 = CARTESIAN_POINT ( 'NONE',  ( 38.01140435219952707, 83.78445800887257633, 34.21067981925357060 ) ) ;
#21376 = CARTESIAN_POINT ( 'NONE',  ( 44.55648932407425633, 102.6844580088725820, 38.96596240072933170 ) ) ;
#21377 = AXIS2_PLACEMENT_3D ( 'NONE', #6553, #16563, #19892 ) ;
#21378 = CARTESIAN_POINT ( 'NONE',  ( 41.46631938032478359, 138.1104996726487286, 29.45539723777780239 ) ) ;
#21380 = CARTESIAN_POINT ( 'NONE',  ( 15.82502354501850483, 112.7224674592991818, 9.875206726065272278 ) ) ;
#21379 = CARTESIAN_POINT ( 'NONE',  ( 44.37947211624943833, 94.01518717409400949, 38.42115945441014446 ) ) ;
#21381 = CARTESIAN_POINT ( 'NONE',  ( 173.3794444120442506, -34.13255853780189142, 5.000000000000018652 ) ) ;
#21382 = CARTESIAN_POINT ( 'NONE',  ( -154.3824083646099439, -163.5584106276440366, 58.62277379824867296 ) ) ;
#21383 = CARTESIAN_POINT ( 'NONE',  ( 38.96631938032478359, 60.41049967264873288, 31.27175355779120025 ) ) ;
#21385 = CARTESIAN_POINT ( 'NONE',  ( 43.80332655382222384, 70.95757658655230671, 29.21067981925357770 ) ) ;
#21384 = FACE_OUTER_BOUND ( 'NONE', #3126, .T. ) ;
#21386 =( NAMED_UNIT ( * ) SI_UNIT ( $, .STERADIAN. ) SOLID_ANGLE_UNIT ( ) );
#21387 = FACE_OUTER_BOUND ( 'NONE', #17882, .T. ) ;
#21388 = CARTESIAN_POINT ( 'NONE',  ( 46.10157429594899270, 79.76049967264873430, 38.46393386101375711 ) ) ;
#21389 = CARTESIAN_POINT ( 'NONE',  ( 41.64333658814960870, 156.9797705074273040, 38.42115945441014446 ) ) ;
#21390 = DIRECTION ( 'NONE',  ( 0.3428981916074309577, -0.9393725726208709270, 0.000000000000000000 ) ) ;
#21391 = VECTOR ( 'NONE', #2431, 1000.000000000000000 ) ;
#21392 = CARTESIAN_POINT ( 'NONE',  ( 43.01140435219951996, 10.71049967264875491, 34.21067981925357060 ) ) ;
#21393 = CARTESIAN_POINT ( 'NONE',  ( -148.5561028927606344, -170.7938272943107165, 40.69124936498395328 ) ) ;
#21394 = CARTESIAN_POINT ( 'NONE',  ( -148.5561028927606344, -180.0584106276440366, 40.69124936498395328 ) ) ;
#21395 = ORIENTED_EDGE ( 'NONE', *, *, #9100, .F. ) ;
#21396 = CARTESIAN_POINT ( 'NONE',  ( 46.59305225739526435, 73.31518717409400665, 36.81289934271958941 ) ) ;
#21397 = CARTESIAN_POINT ( 'NONE',  ( -148.5561028927606344, -165.0584106276440366, 40.69124936498395328 ) ) ;
#21398 = CARTESIAN_POINT ( 'NONE',  ( 12.64719099284060988, 103.9244585094960769, 21.54915782717631600 ) ) ;
#21399 = AXIS2_PLACEMENT_3D ( 'NONE', #12155, #18886, #10085 ) ;
#21400 = CARTESIAN_POINT ( 'NONE',  ( 46.10157429594899270, 111.8344580088725877, 38.46393386101375711 ) ) ;
#21401 = CARTESIAN_POINT ( 'NONE',  ( 44.37947211624943833, 131.2151871740940123, 30.00020018409699318 ) ) ;
#21402 = EDGE_CURVE ( 'NONE', #17102, #4204, #3606, .T. ) ;
#21403 = CARTESIAN_POINT ( 'NONE',  ( 36.18411527879869993, 86.44273942418264767, -5.442340506565031433 ) ) ;
#21404 = ORIENTED_EDGE ( 'NONE', *, *, #1668, .F. ) ;
#21405 = APPLICATION_CONTEXT ( 'automotive_design' ) ;
#21406 = ORIENTED_EDGE ( 'NONE', *, *, #8181, .T. ) ;
#21407 = VECTOR ( 'NONE', #4486, 1000.000000000000000 ) ;
#21408 = CARTESIAN_POINT ( 'NONE',  ( 44.55648932407425633, 116.8104996726487599, 29.45539723777780239 ) ) ;
#21409 = CARTESIAN_POINT ( 'NONE',  ( 38.58424406990784661, 78.22977050742731819, 32.77220824515698183 ) ) ;
#21411 = CARTESIAN_POINT ( 'NONE',  ( 70.03002323795641360, 111.8333997399938511, 5.989792257250448060 ) ) ;
#21410 = CARTESIAN_POINT ( 'NONE',  ( 47.43856463449117200, 124.4651871740939839, 35.64915139335016647 ) ) ;
#21412 = CARTESIAN_POINT ( 'NONE',  ( 47.05648932407426344, 95.51049967264873430, 31.27175355779120025 ) ) ;
#21413 = STYLED_ITEM ( 'NONE', ( #15143 ), #7102 ) ;
#21414 = CARTESIAN_POINT ( 'NONE',  ( 75.59501567365037999, 109.4093883240155378, 12.93430809701916750 ) ) ;
#21415 = CARTESIAN_POINT ( 'NONE',  ( -56.84366818088135176, 789.5005544000622422, -19.99999999999997868 ) ) ;
#21416 = SHAPE_REPRESENTATION ( 'Handle Grip Sleeve', ( #12657 ), #17239 ) ;
#21417 = CARTESIAN_POINT ( 'NONE',  ( 46.59305225739526435, 91.31518717409399244, 36.81289934271958941 ) ) ;
#21418 = CARTESIAN_POINT ( 'NONE',  ( 41.71434717473703557, 144.8754631261027441, 39.05053369627938054 ) ) ;
#21419 = CARTESIAN_POINT ( 'NONE',  ( 43.80332655382222384, 71.88361825032846752, 29.21067981925357770 ) ) ;
#21420 = CARTESIAN_POINT ( 'NONE',  ( 43.01140435219951996, 10.71049967264875491, 39.21067981925356349 ) ) ;
#21421 = ORIENTED_EDGE ( 'NONE', *, *, #12984, .F. ) ;
#21422 = CARTESIAN_POINT ( 'NONE',  ( 44.37947211624943833, 76.27977050742731535, 38.42115945441014446 ) ) ;
#21423 = CARTESIAN_POINT ( 'NONE',  ( -151.4692556286852891, -191.9084106276440025, 39.74470866294723947 ) ) ;
#21424 = CARTESIAN_POINT ( 'NONE',  ( 47.30009524607925897, 85.94413156685014599, 0.1962900075584997628 ) ) ;
#21425 = CARTESIAN_POINT ( 'NONE',  ( -154.3824083646099439, -182.7584106276440536, 40.69124936498395328 ) ) ;
#21426 = ORIENTED_EDGE ( 'NONE', *, *, #1282, .F. ) ;
#21427 = LINE ( 'NONE', #14796, #12175 ) ;
#21428 = DIRECTION ( 'NONE',  ( 0.3450121214752276400, -0.9385982292947087080, -0.000000000000000000 ) ) ;
#21429 = CARTESIAN_POINT ( 'NONE',  ( 45.74753988029934249, 125.3297705074273409, 30.44471234641812174 ) ) ;
#21430 = VERTEX_POINT ( 'NONE', #5357 ) ;
#21431 = DIRECTION ( 'NONE',  ( 0.000000000000000000, -1.000000000000000000, 0.000000000000000000 ) ) ;
#21432 = ORIENTED_EDGE ( 'NONE', *, *, #11333, .T. ) ;
#21433 = CARTESIAN_POINT ( 'NONE',  ( 46.59305225739526435, 119.1797705074273068, 31.60846029578754468 ) ) ;
#21434 = CARTESIAN_POINT ( 'NONE',  ( -158.9748091281504401, -116.9891397928655010, 62.65701158161630957 ) ) ;
#21435 = CARTESIAN_POINT ( 'NONE',  ( 47.05648932407426344, 67.58445800887258770, 31.27175355779120025 ) ) ;
#21436 = CARTESIAN_POINT ( 'NONE',  ( -134.9004869860375777, 755.4811543468929358, -19.99999999999996092 ) ) ;
#21437 = CARTESIAN_POINT ( 'NONE',  ( 41.46631938032478359, 84.38445800887258486, 38.96596240072933170 ) ) ;
#21438 = FILL_AREA_STYLE ('',( #11283 ) ) ;
#21439 = CARTESIAN_POINT ( 'NONE',  ( -151.4692556286852891, -193.7391397928654442, 60.17163382399899518 ) ) ;
#21440 =( BOUNDED_CURVE ( )  B_SPLINE_CURVE ( 2, ( #7468, #2493, #7579, #9452, #13375, #21760, #20112, #8311, #36, #21130, #5003, #6777, #7694 ),
 .UNSPECIFIED., .F., .F. ) 
 B_SPLINE_CURVE_WITH_KNOTS ( ( 3, 2, 2, 2, 2, 2, 3 ),
 ( 0.03676470588235293546, 0.03823529411764706176, 0.04117647058823529355, 0.04411764705882353227, 0.04705882352941176405, 0.05000000000000000278, 0.05147058823529412214 ),
 .UNSPECIFIED. ) 
 CURVE ( )  GEOMETRIC_REPRESENTATION_ITEM ( )  RATIONAL_B_SPLINE_CURVE ( ( 0.9755282581475767101, 0.9755282581475765991, 1.000000000000000000, 0.9510565162951535312, 1.000000000000000000, 0.9510565162951535312, 1.000000000000000000, 0.9510565162951535312, 1.000000000000000000, 0.9510565162951535312, 1.000000000000000000, 0.9755282581475767101, 0.9755282581475768211 ) ) 
 REPRESENTATION_ITEM ( '' )  );
#21441 = CARTESIAN_POINT ( 'NONE',  ( 43.01140435219951996, 157.4604996726487514, 39.21067981925355639 ) ) ;
#21442 = CARTESIAN_POINT ( 'NONE',  ( 131.9510975077307933, 193.6375880255003779, 34.00000000000001421 ) ) ;
#21443 = CARTESIAN_POINT ( 'NONE',  ( -143.8425227516148084, -195.0938272943107279, 44.11586579668791330 ) ) ;
#21444 = AXIS2_PLACEMENT_3D ( 'NONE', #21058, #5938, #9367 ) ;
#21445 = CARTESIAN_POINT ( 'NONE',  ( 38.96631938032478359, 119.4844580088725792, 31.27175355779120025 ) ) ;
#21446 = CARTESIAN_POINT ( 'NONE',  ( 40.27526882409969033, 104.9297705074273210, 30.44471234641811819 ) ) ;
#21447 = CARTESIAN_POINT ( 'NONE',  ( 70.54646159239726444, 126.3605644061445901, 18.41388650843374464 ) ) ;
#21448 = CARTESIAN_POINT ( 'NONE',  ( -159.0959885057557983, -181.5938272943107279, 55.19815736654470584 ) ) ;
#21449 = CARTESIAN_POINT ( 'NONE',  ( 41.64333658814960870, 92.51518717409399528, 30.00020018409699318 ) ) ;
#21450 = DIRECTION ( 'NONE',  ( -0.9385982292947088190, -0.3450121214752278620, 0.000000000000000000 ) ) ;
#21451 = VERTEX_POINT ( 'NONE', #12073 ) ;
#21452 = DIRECTION ( 'NONE',  ( -1.000000000000000000, 0.000000000000000000, 0.000000000000000000 ) ) ;
#21453 = CARTESIAN_POINT ( 'NONE',  ( 17.60877916486148465, 96.95950790538488206, 1.267834678905774393 ) ) ;
#21454 = CARTESIAN_POINT ( 'NONE',  ( 16.34080065753823163, 110.9948608346959276, -11.19624206051981474 ) ) ;
#21455 = EDGE_CURVE ( 'NONE', #7641, #20771, #18642, .T. ) ;
#21456 = CARTESIAN_POINT ( 'NONE',  ( 45.74753988029934249, 70.42977050742730682, 37.97664729208901235 ) ) ;
#21457 = EDGE_LOOP ( 'NONE', ( #20567, #9393, #6571, #11571 ) ) ;
#21458 = ORIENTED_EDGE ( 'NONE', *, *, #16085, .F. ) ;
#21459 = CARTESIAN_POINT ( 'NONE',  ( 39.42975644700377558, 156.0797705074273267, 31.60846029578754468 ) ) ;
#21460 = AXIS2_PLACEMENT_3D ( 'NONE', #13408, #8236, #20141 ) ;
#21461 = DIRECTION ( 'NONE',  ( 0.9385982292947087080, 0.3450121214752278620, -1.836742322155470738E-16 ) ) ;
#21462 = CARTESIAN_POINT ( 'NONE',  ( 48.01140435219951996, 107.0604996726487599, 35.83527830041810347 ) ) ;
#21463 = CARTESIAN_POINT ( 'NONE',  ( 43.01140435219951286, 65.36518717409400381, 29.55568802177586463 ) ) ;
#21464 = CARTESIAN_POINT ( 'NONE',  ( 43.01140435219951286, 65.03445800887257633, 29.21067981925356705 ) ) ;
#21465 = CARTESIAN_POINT ( 'NONE',  ( -159.0959885057557983, -160.5938272943107279, 55.19815736654470584 ) ) ;
#21466 = CARTESIAN_POINT ( 'NONE',  ( 163.2444732741424787, 192.0234091111227883, 19.84828153075611823 ) ) ;
#21467 = CARTESIAN_POINT ( 'NONE',  ( -145.2889157411863721, -174.5130981290892578, 58.16351966513671812 ) ) ;
#21468 = DIRECTION ( 'NONE',  ( 0.000000000000000000, 0.000000000000000000, 1.000000000000000000 ) ) ;
#21469 = EDGE_CURVE ( 'NONE', #17427, #1334, #17223, .T. ) ;
#21470 = CARTESIAN_POINT ( 'NONE',  ( 46.10157429594899270, 148.7344580088725934, 29.95742577749337343 ) ) ;
#21471 = CARTESIAN_POINT ( 'NONE',  ( 44.37947211624943833, 133.2797705074273154, 38.42115945441014446 ) ) ;
#21472 = CARTESIAN_POINT ( 'NONE',  ( 69.75981547520746062, 141.4021063757441823, 10.83457600654633879 ) ) ;
#21473 = CARTESIAN_POINT ( 'NONE',  ( 40.27526882409969744, 120.5651871740940209, 37.97664729208901235 ) ) ;
#21474 = LINE ( 'NONE', #20156, #3021 ) ;
#21475 = DIRECTION ( 'NONE',  ( 0.000000000000000000, 0.000000000000000000, 1.000000000000000000 ) ) ;
#21476 = PRODUCT_DEFINITION_FORMATION_WITH_SPECIFIED_SOURCE ( 'ANY', '', #8013, .NOT_KNOWN. ) ;
#21477 = EDGE_CURVE ( 'NONE', #20292, #12851, #6379, .T. ) ;
#21478 = CARTESIAN_POINT ( 'NONE',  ( 48.01140435219951996, 140.0604996726487457, 35.83527830041809636 ) ) ;
#21479 = LINE ( 'NONE', #16174, #9942 ) ;
#21480 = EDGE_CURVE ( 'NONE', #2927, #16287, #18166, .T. ) ;
#21481 = CARTESIAN_POINT ( 'NONE',  ( 65.38103680468944390, 137.2114283014329317, 17.93782343147312730 ) ) ;
#21482 = CARTESIAN_POINT ( 'NONE',  ( 43.01140435219951996, 10.71049967264875491, 29.21067981925357060 ) ) ;
#21483 = ORIENTED_EDGE ( 'NONE', *, *, #15154, .T. ) ;
#21484 = EDGE_CURVE ( 'NONE', #6341, #18099, #17675, .T. ) ;
#21485 = CARTESIAN_POINT ( 'NONE',  ( -149.8854112254399240, -156.3160212151857422, 39.65701158161629536 ) ) ;
#21486 = ORIENTED_EDGE ( 'NONE', *, *, #12200, .T. ) ;
#21487 = CARTESIAN_POINT ( 'NONE',  ( 38.96631938032478359, 81.08445800887258770, 37.14960608071593384 ) ) ;
#21488 = DIRECTION ( 'NONE',  ( 1.000000000000000000, 0.000000000000000000, -1.648795714028702312E-16 ) ) ;
#21489 = VECTOR ( 'NONE', #18187, 1000.000000000000000 ) ;
#21490 = CARTESIAN_POINT ( 'NONE',  ( 39.92123440845004723, 139.1604996726487400, 38.46393386101376421 ) ) ;
#21492 = CARTESIAN_POINT ( 'NONE',  ( 68.61421220432494295, 108.2796574941523886, 7.137043325852385323 ) ) ;
#21491 = CARTESIAN_POINT ( 'NONE',  ( 44.37947211624943833, 98.21518717409399812, 30.00020018409699318 ) ) ;
#21493 = CARTESIAN_POINT ( 'NONE',  ( -154.3824083646099439, -170.7584106276440536, 40.69124936498395328 ) ) ;
#21494 = CARTESIAN_POINT ( 'NONE',  ( -148.5561028927606344, -191.7938272943107449, 40.69124936498395328 ) ) ;
#21496 = DIRECTION ( 'NONE',  ( 0.000000000000000000, 1.000000000000000000, 0.000000000000000000 ) ) ;
#21495 = LINE ( 'NONE', #6497, #1663 ) ;
#21497 = CARTESIAN_POINT ( 'NONE',  ( -145.2889157411863437, -188.6130981290893374, 41.15050349809589392 ) ) ;
#21498 = EDGE_CURVE ( 'NONE', #17801, #14823, #7131, .T. ) ;
#21499 = CARTESIAN_POINT ( 'NONE',  ( -151.4692556286853176, -175.7391397928654726, 59.65701158161632378 ) ) ;
#21500 = CARTESIAN_POINT ( 'NONE',  ( 48.01140435219951996, 115.2844580088725763, 34.21067981925357060 ) ) ;
#21501 = CARTESIAN_POINT ( 'NONE',  ( 47.43856463449117200, 61.76518717409399528, 32.77220824515698183 ) ) ;
#21502 = FACE_OUTER_BOUND ( 'NONE', #15333, .T. ) ;
#21503 = CARTESIAN_POINT ( 'NONE',  ( 32.14050509837299785, 87.44534670509604268, 7.696117750009315195 ) ) ;
#21504 = CARTESIAN_POINT ( 'NONE',  ( 40.27526882409969744, 153.5651871740940067, 37.97664729208901235 ) ) ;
#21505 = CARTESIAN_POINT ( 'NONE',  ( -145.6429501568359797, -158.9438272943107222, 41.63779006702063867 ) ) ;
#21506 = CARTESIAN_POINT ( 'NONE',  ( -159.0959885057557983, -187.8584106276440480, 55.19815736654470584 ) ) ;
#21507 = EDGE_CURVE ( 'NONE', #4221, #460, #14158, .T. ) ;
#21508 = EDGE_LOOP ( 'NONE', ( #5641, #15440, #19761, #14355 ) ) ;
#21509 = CARTESIAN_POINT ( 'NONE',  ( 44.37947211624943833, 71.21518717409399812, 30.00020018409699318 ) ) ;
#21510 =( BOUNDED_CURVE ( )  B_SPLINE_CURVE ( 2, ( #8054, #8974, #908, #17654, #4006, #10846, #16116, #7430, #11044, #584, #17760, #2662, #17543 ),
 .UNSPECIFIED., .F., .F. ) 
 B_SPLINE_CURVE_WITH_KNOTS ( ( 3, 2, 2, 2, 2, 2, 3 ),
 ( 0.8392857142857143016, 0.8428571428571428603, 0.8499999999999999778, 0.8571428571428570953, 0.8642857142857143238, 0.8714285714285714413, 0.8750000000000000000 ),
 .UNSPECIFIED. ) 
 CURVE ( )  GEOMETRIC_REPRESENTATION_ITEM ( )  RATIONAL_B_SPLINE_CURVE ( ( 0.9755282581475768211, 0.9755282581475768211, 1.000000000000000000, 0.9510565162951535312, 1.000000000000000000, 0.9510565162951535312, 1.000000000000000000, 0.9510565162951535312, 1.000000000000000000, 0.9510565162951535312, 1.000000000000000000, 0.9755282581475768211, 0.9755282581475768211 ) ) 
 REPRESENTATION_ITEM ( '' )  );
#21511 = CARTESIAN_POINT ( 'NONE',  ( -148.5561028927606344, -168.0584106276440366, 40.69124936498395328 ) ) ;
#21512 = CARTESIAN_POINT ( 'NONE',  ( 75.41016232129729246, 131.2110917358880045, 18.21592158385217886 ) ) ;
#21513 = CARTESIAN_POINT ( 'NONE',  ( 47.05648932407426344, 112.5844580088725877, 31.27175355779120025 ) ) ;
#21514 = CARTESIAN_POINT ( 'NONE',  ( 45.74753988029933538, 134.0651871740939498, 30.44471234641811819 ) ) ;
#21515 = CARTESIAN_POINT ( 'NONE',  ( 13.29607544193514990, 103.0715419909171970, -4.489867183945484896 ) ) ;
#21516 = EDGE_LOOP ( 'NONE', ( #570, #9933, #17074, #7501 ) ) ;
#21517 = EDGE_LOOP ( 'NONE', ( #20884, #6752, #93, #7767 ) ) ;
#21518 = CARTESIAN_POINT ( 'NONE',  ( 15.16534570839878349, 115.4582699162533288, 15.98979919289822149 ) ) ;
#21519 = EDGE_LOOP ( 'NONE', ( #13558, #1165, #18665, #7330 ) ) ;
#21520 = EDGE_CURVE ( 'NONE', #19975, #4439, #19822, .T. ) ;
#21521 = CARTESIAN_POINT ( 'NONE',  ( 43.01140435219951996, 10.71049967264875491, 39.21067981925356349 ) ) ;
#21522 = CARTESIAN_POINT ( 'NONE',  ( 41.64333658814960870, 71.77977050742731535, 30.00020018409699318 ) ) ;
#21524 = CARTESIAN_POINT ( 'NONE',  ( 55.81398226145393693, 145.0329042473489096, 4.442248136324586483 ) ) ;
#21523 = CARTESIAN_POINT ( 'NONE',  ( 46.59305225739526435, 124.9151871740940010, 31.60846029578754468 ) ) ;
#21525 = CARTESIAN_POINT ( 'NONE',  ( 38.96631938032478359, 82.01049967264874851, 37.14960608071593384 ) ) ;
#21526 = CARTESIAN_POINT ( 'NONE',  ( 19.13088699441526686, 95.37848931739559077, 15.19637875606281341 ) ) ;
#21527 = LINE ( 'NONE', #8191, #6213 ) ;
#21528 = CARTESIAN_POINT ( 'NONE',  ( 47.43856463449117200, 91.76518717409400949, 32.77220824515698183 ) ) ;
#21529 = MANIFOLD_SOLID_BREP ( 'Boss-Extrude4', #375 ) ;
#21530 = CARTESIAN_POINT ( 'NONE',  ( 48.01140435219951996, 151.1344580088725991, 35.83527830041809636 ) ) ;
#21531 = CARTESIAN_POINT ( 'NONE',  ( 44.55648932407425633, 141.6844580088725820, 38.96596240072933170 ) ) ;
#21532 = ORIENTED_EDGE ( 'NONE', *, *, #17428, .T. ) ;
#21533 = CARTESIAN_POINT ( 'NONE',  ( 46.59305225739526435, 65.17977050742732104, 31.60846029578754468 ) ) ;
#21534 = CARTESIAN_POINT ( 'NONE',  ( -156.1828684652451500, -155.3945645429188005, 41.49287016839741682 ) ) ;
#21535 = CARTESIAN_POINT ( 'NONE',  ( 41.61242760320212852, 154.1118385459532760, 10.79173905232880237 ) ) ;
#21536 = CARTESIAN_POINT ( 'NONE',  ( -143.8425227516148084, -180.9584106276440707, 55.19815736654470584 ) ) ;
#21537 = ORIENTED_EDGE ( 'NONE', *, *, #21520, .F. ) ;
#21538 = CARTESIAN_POINT ( 'NONE',  ( -91.10645082872859746, 10.96617311717548660, -19.99999999999997868 ) ) ;
#21539 = CARTESIAN_POINT ( 'NONE',  ( 38.58424406990785371, 126.5297705074272869, 35.64915139335015937 ) ) ;
#21540 = ORIENTED_EDGE ( 'NONE', *, *, #6235, .F. ) ;
#21541 = CARTESIAN_POINT ( 'NONE',  ( 43.01140435219951286, 129.5344580088725763, 39.21067981925356349 ) ) ;
#21542 = ORIENTED_EDGE ( 'NONE', *, *, #1506, .T. ) ;
#21543 = CARTESIAN_POINT ( 'NONE',  ( 46.59305225739526435, 118.5797705074273267, 36.81289934271958941 ) ) ;
#21544 = DIRECTION ( 'NONE',  ( 0.2767211344570353337, -0.9609502660100633920, 0.000000000000000000 ) ) ;
#21545 = CARTESIAN_POINT ( 'NONE',  ( 46.59305225739526435, 151.3151871740940067, 36.81289934271958941 ) ) ;
#21546 = EDGE_CURVE ( 'NONE', #4098, #10985, #12286, .T. ) ;
#21547 = AXIS2_PLACEMENT_3D ( 'NONE', #6775, #20214, #3461 ) ;
#21548 = DIRECTION ( 'NONE',  ( 0.000000000000000000, 1.000000000000000000, 0.000000000000000000 ) ) ;
#21549 = CARTESIAN_POINT ( 'NONE',  ( 38.96631938032478359, 84.08445800887258770, 37.14960608071593384 ) ) ;
#21550 = CARTESIAN_POINT ( 'NONE',  ( 42.21948215057684450, 96.03738109496902098, 29.21067981925356705 ) ) ;
#21551 = CARTESIAN_POINT ( 'NONE',  ( -143.3790856849358306, -183.6891397928654612, 43.77915905869157598 ) ) ;
#21552 = CARTESIAN_POINT ( 'NONE',  ( 91.17254549292282206, -61.68114226949890622, 20.00000000000001776 ) ) ;
#21553 = CARTESIAN_POINT ( 'NONE',  ( 44.55648932407425633, 131.8104996726487457, 29.45539723777780239 ) ) ;
#21554 = CARTESIAN_POINT ( 'NONE',  ( -151.4692556286852891, -187.1438272943106824, 59.56931450028537967 ) ) ;
#21555 = CONTEXT_DEPENDENT_SHAPE_REPRESENTATION ( #20981, #18022 ) ;
#21556 = CIRCLE ( 'NONE', #12041, 27.14138364107347812 ) ;
#21557 = CARTESIAN_POINT ( 'NONE',  ( 38.01140435219951996, 125.9344580088725962, 35.83527830041810347 ) ) ;
#21558 = CARTESIAN_POINT ( 'NONE',  ( 43.01140435219951286, 107.6297705074272955, 29.55568802177586463 ) ) ;
#21559 = CARTESIAN_POINT ( 'NONE',  ( 58.78870511939484800, 143.3781512503299780, 17.58070913143554748 ) ) ;
#21560 = CARTESIAN_POINT ( 'NONE',  ( -154.3824083646099439, -179.4938272943107336, 40.69124936498395328 ) ) ;
#21561 = CARTESIAN_POINT ( 'NONE',  ( 38.58424406990785371, 87.26518717409399528, 35.64915139335015937 ) ) ;
#21562 = CARTESIAN_POINT ( 'NONE',  ( 43.01140435219951996, 10.71049967264875491, 39.21067981925356349 ) ) ;
#21563 = ORIENTED_EDGE ( 'NONE', *, *, #10473, .F. ) ;
#21564 = CARTESIAN_POINT ( 'NONE',  ( 70.26356658872128946, 140.6255928306487704, 11.86290872716119615 ) ) ;
#21565 = CARTESIAN_POINT ( 'NONE',  ( 38.58424406990785371, 144.2297705074273324, 32.77220824515697473 ) ) ;
#21566 = CARTESIAN_POINT ( 'NONE',  ( 49.32098446784893753, 92.50438258598539676, -5.839070001793449372 ) ) ;
#21567 = PRODUCT ( 'Handle Grip Sleeve', 'Handle Grip Sleeve', '', ( #9654 ) ) ;
#21568 = CARTESIAN_POINT ( 'NONE',  ( 45.74753988029934249, 62.32977050742730540, 30.44471234641812174 ) ) ;
#21569 = ORIENTED_EDGE ( 'NONE', *, *, #7039, .T. ) ;
#21570 = ORIENTED_EDGE ( 'NONE', *, *, #19064, .T. ) ;
#21571 = CARTESIAN_POINT ( 'NONE',  ( 47.43856463449117200, 149.0297705074273438, 32.77220824515698183 ) ) ;
#21572 = LINE ( 'NONE', #6352, #4906 ) ;
#21573 = CARTESIAN_POINT ( 'NONE',  ( 38.96631938032478359, 109.0104996726487485, 37.14960608071593384 ) ) ;
#21574 = CARTESIAN_POINT ( 'NONE',  ( 38.58424406990784661, 72.26518717409398107, 35.64915139335016647 ) ) ;
#21575 = CARTESIAN_POINT ( 'NONE',  ( -145.6429501568359797, -156.2084106276440423, 41.63779006702063867 ) ) ;
#21576 = CARTESIAN_POINT ( 'NONE',  ( -157.2955611005345986, -158.3438272943106995, 41.63779006702063867 ) ) ;
#21577 = LINE ( 'NONE', #21798, #5462 ) ;
#21578 = CARTESIAN_POINT ( 'NONE',  ( -154.5594255724347761, -180.9630981290893033, 59.16757674456785310 ) ) ;
#21579 =( LENGTH_UNIT ( ) NAMED_UNIT ( * ) SI_UNIT ( .MILLI., .METRE. ) );
#21580 = CARTESIAN_POINT ( 'NONE',  ( 41.46631938032478359, 112.3104996726487457, 38.96596240072933170 ) ) ;
#21582 = EDGE_CURVE ( 'NONE', #18977, #19943, #2498, .T. ) ;
#21581 = CARTESIAN_POINT ( 'NONE',  ( 44.55648932407425633, 147.6844580088725820, 38.96596240072933170 ) ) ;
#21583 = CARTESIAN_POINT ( 'NONE',  ( 45.74753988029933538, 134.3297705074273267, 30.44471234641811819 ) ) ;
#21584 = CARTESIAN_POINT ( 'NONE',  ( 10.15219960346482431, 110.0225462658725490, 14.76332465322822074 ) ) ;
#21585 = CARTESIAN_POINT ( 'NONE',  ( 39.42975644700377558, 116.8151871740940067, 31.60846029578754468 ) ) ;
#21586 = CARTESIAN_POINT ( 'NONE',  ( -159.5594255724347761, -167.7891397928654840, 43.77915905869157598 ) ) ;
#21587 = DIRECTION ( 'NONE',  ( 0.000000000000000000, 1.000000000000000000, 0.000000000000000000 ) ) ;
#21588 = CARTESIAN_POINT ( 'NONE',  ( -79.69854755000110913, 605.3054376597395958, -19.99999999999996092 ) ) ;
#21589 = CARTESIAN_POINT ( 'NONE',  ( 52.64611633815218283, 152.6728927476294189, 5.153103026933554709 ) ) ;
#21590 = CARTESIAN_POINT ( 'NONE',  ( 26.61521700243209310, 142.9206948758876194, 23.22567064538713666 ) ) ;
#21591 = PRODUCT_RELATED_PRODUCT_CATEGORY ( 'part', '', ( #9956 ) ) ;
#21592 = CARTESIAN_POINT ( 'NONE',  ( -141.4692556286852891, -186.8391397928654669, 46.40781461928724383 ) ) ;
#21593 = CARTESIAN_POINT ( 'NONE',  ( 46.59305225739526435, 98.17977050742732104, 31.60846029578754468 ) ) ;
#21594 = VERTEX_POINT ( 'NONE', #15596 ) ;
#21595 = EDGE_CURVE ( 'NONE', #11010, #14442, #13765, .T. ) ;
#21596 = CARTESIAN_POINT ( 'NONE',  ( -151.4692556286852891, -196.9891397928655010, 58.65701158161631668 ) ) ;
#21597 = ORIENTED_EDGE ( 'NONE', *, *, #7368, .F. ) ;
#21598 = EDGE_CURVE ( 'NONE', #17748, #13406, #3024, .T. ) ;
#21599 = CARTESIAN_POINT ( 'NONE',  ( 46.10157429594899270, 78.83445800887255928, 38.46393386101376421 ) ) ;
#21600 = CARTESIAN_POINT ( 'NONE',  ( 43.01140435219951286, 102.5344580088725763, 39.21067981925356349 ) ) ;
#21601 = CARTESIAN_POINT ( 'NONE',  ( 38.96631938032478359, 144.4104996726487400, 31.27175355779120025 ) ) ;
#21603 = CARTESIAN_POINT ( 'NONE',  ( 16.85323768375146614, 130.1535925207217588, 10.57871716905499682 ) ) ;
#21602 = CARTESIAN_POINT ( 'NONE',  ( 39.42975644700377558, 92.81518717409399244, 31.60846029578754468 ) ) ;
#21604 = EDGE_CURVE ( 'NONE', #19734, #19257, #16457, .T. ) ;
#21605 = CARTESIAN_POINT ( 'NONE',  ( -151.4692556286852891, -167.9084106276440309, 39.74470866294723947 ) ) ;
#21606 = CARTESIAN_POINT ( 'NONE',  ( -160.8964159109769696, -187.7438272943107336, 52.72008163687743121 ) ) ;
#21608 = PLANE ( 'NONE',  #17457 ) ;
#21607 = CARTESIAN_POINT ( 'NONE',  ( -157.6495955161842062, -178.1130981290893089, 58.16351966513671812 ) ) ;
#21609 = DIRECTION ( 'NONE',  ( -0.000000000000000000, -0.000000000000000000, 1.000000000000000000 ) ) ;
#21610 = CARTESIAN_POINT ( 'NONE',  ( -143.3790856849358306, -175.2891397928654840, 55.53486410454105027 ) ) ;
#21611 = DIRECTION ( 'NONE',  ( -1.000000000000000000, 0.000000000000000000, 1.186952418100008737E-16 ) ) ;
#21612 = CARTESIAN_POINT ( 'NONE',  ( 43.01140435219951286, 63.86518717409398960, 38.86567161673127657 ) ) ;
#21613 = CARTESIAN_POINT ( 'NONE',  ( -157.6495955161842062, -185.0130981290893146, 41.15050349809589392 ) ) ;
#21614 = CARTESIAN_POINT ( 'NONE',  ( 71.53613896966024299, 138.8348963267899592, -2.065403804986401859 ) ) ;
#21615 = CARTESIAN_POINT ( 'NONE',  ( 38.58424406990785371, 149.9651871740939555, 32.77220824515697473 ) ) ;
#21616 = CARTESIAN_POINT ( 'NONE',  ( -157.2955611005346270, -158.3438272943106995, 41.63779006702063867 ) ) ;
#21617 = CARTESIAN_POINT ( 'NONE',  ( -157.2955611005345986, -182.6084106276440480, 41.63779006702063867 ) ) ;
#21618 = VERTEX_POINT ( 'NONE', #19551 ) ;
#21619 = CARTESIAN_POINT ( 'NONE',  ( 45.74753988029934249, 71.06518717409400665, 30.44471234641812174 ) ) ;
#21620 = CARTESIAN_POINT ( 'NONE',  ( -157.2955611005346270, -170.6084106276440480, 41.63779006702063867 ) ) ;
#21621 = CARTESIAN_POINT ( 'NONE',  ( 77.30322022806339533, 121.1324128411339984, 11.54915785461027511 ) ) ;
#21622 =( LENGTH_UNIT ( ) NAMED_UNIT ( * ) SI_UNIT ( .MILLI., .METRE. ) );
#21623 = CARTESIAN_POINT ( 'NONE',  ( 47.43856463449118621, 127.6151871740940038, 34.21067981925357060 ) ) ;
#21624 = CARTESIAN_POINT ( 'NONE',  ( 8.857566569312460558, 119.8222194325741725, -10.91815776494309098 ) ) ;
#21625 = EDGE_LOOP ( 'NONE', ( #7929, #14036 ) ) ;
#21626 = ORIENTED_EDGE ( 'NONE', *, *, #17590, .T. ) ;
#21627 = VECTOR ( 'NONE', #16717, 1000.000000000000000 ) ;
#21628 = CARTESIAN_POINT ( 'NONE',  ( -149.8854112254399240, -192.3160212151857422, 39.65701158161631668 ) ) ;
#21629 = EDGE_LOOP ( 'NONE', ( #2331, #12142, #15191, #10955 ) ) ;
#21630 = CARTESIAN_POINT ( 'NONE',  ( 44.55648932407425633, 106.8844580088725849, 29.45539723777780239 ) ) ;
#21631 = CARTESIAN_POINT ( 'NONE',  ( -151.4692556286852891, -195.9891397928654726, 49.65701158161630957 ) ) ;
#21632 = CARTESIAN_POINT ( 'NONE',  ( 45.74753988029933538, 68.32977050742731251, 30.44471234641811819 ) ) ;
#21634 = CARTESIAN_POINT ( 'NONE',  ( 45.98873144221455789, 91.86516812052268222, 7.299390993452533394 ) ) ;
#21633 = CARTESIAN_POINT ( 'NONE',  ( 47.43856463449117200, 121.7651871740940237, 32.77220824515698183 ) ) ;
#21635 = VECTOR ( 'NONE', #858, 1000.000000000000000 ) ;
#21636 = CARTESIAN_POINT ( 'NONE',  ( 48.01140435219951996, 86.21049967264873715, 34.21067981925357060 ) ) ;
#21637 = LINE ( 'NONE', #13249, #17445 ) ;
#21638 = CARTESIAN_POINT ( 'NONE',  ( -151.4692556286852607, -170.3130981290892692, 39.65701158161629536 ) ) ;
#21639 = CARTESIAN_POINT ( 'NONE',  ( 147.5268905834513475, 193.0332408774651185, -50.99999999999998579 ) ) ;
#21640 =( BOUNDED_CURVE ( )  B_SPLINE_CURVE ( 2, ( #994, #4396, #14324, #19397, #11128, #4293, #10034, #3422, #16630, #11783, #18062, #16409, #5281 ),
 .UNSPECIFIED., .F., .F. ) 
 B_SPLINE_CURVE_WITH_KNOTS ( ( 3, 2, 2, 2, 2, 2, 3 ),
 ( 0.1250000000000000000, 0.1264705882352941124, 0.1294117647058823650, 0.1323529411764705899, 0.1352941176470588147, 0.1382352941176470673, 0.1397058823529411797 ),
 .UNSPECIFIED. ) 
 CURVE ( )  GEOMETRIC_REPRESENTATION_ITEM ( )  RATIONAL_B_SPLINE_CURVE ( ( 0.9755282581475768211, 0.9755282581475768211, 1.000000000000000000, 0.9510565162951535312, 1.000000000000000000, 0.9510565162951535312, 1.000000000000000000, 0.9510565162951535312, 1.000000000000000000, 0.9510565162951535312, 1.000000000000000000, 0.9755282581475768211, 0.9755282581475768211 ) ) 
 REPRESENTATION_ITEM ( '' )  );
#21641 = CARTESIAN_POINT ( 'NONE',  ( 43.01140435219951286, 86.36518717409400381, 29.55568802177586463 ) ) ;
#21642 = CARTESIAN_POINT ( 'NONE',  ( 38.01127636974734259, 144.4019489221308277, 33.88560042642480141 ) ) ;
#21643 = CARTESIAN_POINT ( 'NONE',  ( 46.10157429594899270, 62.66049967264872578, 29.95742577749336988 ) ) ;
#21644 = ORIENTED_EDGE ( 'NONE', *, *, #1717, .T. ) ;
#21645 = CARTESIAN_POINT ( 'NONE',  ( 45.74753988029933538, 70.42977050742730682, 37.97664729208901946 ) ) ;
#21646 = CARTESIAN_POINT ( 'NONE',  ( -143.8425227516148084, -156.0938272943107279, 44.11586579668791330 ) ) ;
#21647 = CARTESIAN_POINT ( 'NONE',  ( 77.22939692449374149, 120.9137088693742044, 5.553548964694690504 ) ) ;
#21648 = CARTESIAN_POINT ( 'NONE',  ( -143.8425227516148084, -189.3584106276440480, 44.11586579668791330 ) ) ;
#21649 = ORIENTED_EDGE ( 'NONE', *, *, #8984, .F. ) ;
#21650 = CARTESIAN_POINT ( 'NONE',  ( 44.37947211624943833, 151.0151871740940237, 38.42115945441014446 ) ) ;
#21651 = LINE ( 'NONE', #4884, #8872 ) ;
#21652 = AXIS2_PLACEMENT_3D ( 'NONE', #16165, #2404, #2611 ) ;
#21653 = CARTESIAN_POINT ( 'NONE',  ( 43.01140435219951286, 113.6297705074273097, 29.55568802177586107 ) ) ;
#21654 = CARTESIAN_POINT ( 'NONE',  ( 66.89036333300305159, 144.4373801540182569, -2.303882249869787291 ) ) ;
#21655 = ORIENTED_EDGE ( 'NONE', *, *, #13389, .F. ) ;
#21656 = EDGE_CURVE ( 'NONE', #561, #20206, #5268, .T. ) ;
#21657 = CARTESIAN_POINT ( 'NONE',  ( 135.5718357590524192, 174.6787949867965324, 14.00000000000001776 ) ) ;
#21658 = ORIENTED_EDGE ( 'NONE', *, *, #15302, .F. ) ;
#21659 = CARTESIAN_POINT ( 'NONE',  ( 45.74753988029933538, 121.4297705074273068, 37.97664729208901946 ) ) ;
#21660 = CARTESIAN_POINT ( 'NONE',  ( 39.92123440845005433, 73.16049967264872578, 38.46393386101375711 ) ) ;
#21661 = CARTESIAN_POINT ( 'NONE',  ( 47.43856463449117200, 154.7651871740940237, 32.77220824515698183 ) ) ;
#21662 = CARTESIAN_POINT ( 'NONE',  ( 9.345857484954766647, 125.6588058825717837, 10.27205150250232535 ) ) ;
#21663 = CARTESIAN_POINT ( 'NONE',  ( -134.9004869860375777, 755.4811543468929358, -3.999999999999980904 ) ) ;
#21664 = CARTESIAN_POINT ( 'NONE',  ( 101.6431471920911207, 239.2647937927896464, 4.000000000000021316 ) ) ;
#21665 = CARTESIAN_POINT ( 'NONE',  ( 173.3794444120442506, -126.9891397928655010, 30.00000000000000000 ) ) ;
#21666 = CARTESIAN_POINT ( 'NONE',  ( -159.5594255724347761, -182.7891397928654840, 43.77915905869157598 ) ) ;
#21667 = DIRECTION ( 'NONE',  ( -1.000000000000000000, 0.000000000000000000, 0.000000000000000000 ) ) ;
#21668 = CARTESIAN_POINT ( 'NONE',  ( 45.22505347682923116, 59.38050100342834270, 30.37668637662395099 ) ) ;
#21669 = CARTESIAN_POINT ( 'NONE',  ( -143.8425227516148084, -189.6938272943107222, 55.19815736654470584 ) ) ;
#21670 = CARTESIAN_POINT ( 'NONE',  ( 38.96631938032478359, 123.0844580088725735, 37.14960608071593384 ) ) ;
#21671 = CARTESIAN_POINT ( 'NONE',  ( 46.59305225739526435, 97.57977050742731251, 36.81289934271958941 ) ) ;
#21672 = CARTESIAN_POINT ( 'NONE',  ( 16.98434641657835797, 108.8433182140206270, 14.72356627441054755 ) ) ;
#21673 = CARTESIAN_POINT ( 'NONE',  ( -159.0959885057557983, -188.1938272943107222, 44.11586579668791330 ) ) ;
#21674 = CARTESIAN_POINT ( 'NONE',  ( 137.5268905834513191, 193.0332408774651185, -49.99999999999997158 ) ) ;
#21675 = AXIS2_PLACEMENT_3D ( 'NONE', #15513, #13957, #15612 ) ;
#21676 = ORIENTED_EDGE ( 'NONE', *, *, #13923, .F. ) ;
#21677 = DIRECTION ( 'NONE',  ( -0.000000000000000000, -0.000000000000000000, -1.000000000000000000 ) ) ;
#21678 = CARTESIAN_POINT ( 'NONE',  ( 12.61881386508366809, 104.1535352963828984, 15.55354899318430739 ) ) ;
#21679 = CARTESIAN_POINT ( 'NONE',  ( 45.74753988029934249, 140.3297705074273267, 30.44471234641812174 ) ) ;
#21680 = CARTESIAN_POINT ( 'NONE',  ( 41.47717036631702570, 147.9855288695934803, -2.148757419388624523 ) ) ;
#21681 = EDGE_CURVE ( 'NONE', #4525, #19770, #14479, .T. ) ;
#21682 = CARTESIAN_POINT ( 'NONE',  ( 38.58424406990785371, 69.52977050742730114, 35.64915139335015937 ) ) ;
#21683 = ORIENTED_EDGE ( 'NONE', *, *, #12699, .T. ) ;
#21684 = CARTESIAN_POINT ( 'NONE',  ( 44.37947211624943833, 145.2797705074273154, 38.42115945441014446 ) ) ;
#21685 = CARTESIAN_POINT ( 'NONE',  ( 43.01140435219951286, 152.9604996726487798, 29.21067981925356705 ) ) ;
#21686 = CARTESIAN_POINT ( 'NONE',  ( 44.55648932407425633, 107.8104996726487457, 29.45539723777780239 ) ) ;
#21687 = CARTESIAN_POINT ( 'NONE',  ( 47.43856463449117200, 70.76518717409399528, 32.77220824515698183 ) ) ;
#21688 = CARTESIAN_POINT ( 'NONE',  ( 38.96631938032478359, 96.08445800887258770, 37.14960608071593384 ) ) ;
#21689 = CARTESIAN_POINT ( 'NONE',  ( -145.6429501568359797, -164.9438272943106938, 41.63779006702063867 ) ) ;
#21690 = CARTESIAN_POINT ( 'NONE',  ( 38.96631938032478359, 156.0844580088725877, 37.14960608071593384 ) ) ;
#21691 = CARTESIAN_POINT ( 'NONE',  ( -141.4692556286852891, -180.2130981290893033, 52.90620854394536821 ) ) ;
#21692 = CARTESIAN_POINT ( 'NONE',  ( -154.5594255724347761, -192.0891397928654953, 40.14644641866476604 ) ) ;
#21693 = CARTESIAN_POINT ( 'NONE',  ( 48.01140435219951996, 154.2844580088725763, 34.21067981925357060 ) ) ;
#21694 = CARTESIAN_POINT ( 'NONE',  ( 46.59305225739526435, 125.1797705074273210, 31.60846029578754468 ) ) ;
#21695 = CARTESIAN_POINT ( 'NONE',  ( 68.49994877969884044, 96.93213776073638144, 19.40600457995573080 ) ) ;
#21696 = CARTESIAN_POINT ( 'NONE',  ( 43.01140435219951286, 113.3651871740939754, 29.55568802177586107 ) ) ;
#21697 = DIRECTION ( 'NONE',  ( 1.000000000000000000, 0.000000000000000000, 0.000000000000000000 ) ) ;
#21698 = CARTESIAN_POINT ( 'NONE',  ( 47.05648932407426344, 65.51049967264874851, 31.27175355779120025 ) ) ;
#21699 = CARTESIAN_POINT ( 'NONE',  ( 48.37701604703377001, 153.6359454806530778, -1.989754116034292197 ) ) ;
#21700 = CARTESIAN_POINT ( 'NONE',  ( 17.48807464456866256, 131.8965856249792523, 2.656420782620954935 ) ) ;
#21701 = PRODUCT_DEFINITION_SHAPE ( 'NONE', 'NONE',  #8538 ) ;
#21702 = CARTESIAN_POINT ( 'NONE',  ( 45.74753988029934249, 97.42977050742730682, 37.97664729208901235 ) ) ;
#21703 = ORIENTED_EDGE ( 'NONE', *, *, #15831, .T. ) ;
#21704 = DIRECTION ( 'NONE',  ( -0.8835682276357670339, -0.4683024526015100442, 0.000000000000000000 ) ) ;
#21705 = VERTEX_POINT ( 'NONE', #4674 ) ;
#21706 = CARTESIAN_POINT ( 'NONE',  ( 39.92123440845004723, 84.23445800887256496, 38.46393386101376421 ) ) ;
#21707 = CARTESIAN_POINT ( 'NONE',  ( 42.21948215057684450, 87.45757658655232092, 39.21067981925355639 ) ) ;
#21708 = MANIFOLD_SOLID_BREP ( 'Boss-Extrude7', #8475 ) ;
#21709 = CARTESIAN_POINT ( 'NONE',  ( 43.01140435219951286, 134.9604996726487514, 28.95336869806222779 ) ) ;
#21711 = CARTESIAN_POINT ( 'NONE',  ( 28.48261614285185672, 95.83124311379776827, 2.017784757223194170 ) ) ;
#21710 = CARTESIAN_POINT ( 'NONE',  ( 38.58424406990786082, 96.11518717409400381, 34.21067981925357060 ) ) ;
#21712 = AXIS2_PLACEMENT_3D ( 'NONE', #10061, #5409, #10277 ) ;
#21713 = CARTESIAN_POINT ( 'NONE',  ( -160.8964159109769696, -164.1584106276440593, 49.65701158161630957 ) ) ;
#21714 = CARTESIAN_POINT ( 'NONE',  ( -142.0420953463936087, -186.3938272943107393, 49.65701158161630957 ) ) ;
#21715 = CARTESIAN_POINT ( 'NONE',  ( 43.01140435219951996, 119.9070776186055838, 50.00000000000002842 ) ) ;
#21716 = CARTESIAN_POINT ( 'NONE',  ( 147.5268905834513475, 193.0332408774651185, -50.99999999999998579 ) ) ;
#21717 = COLOUR_RGB ( '', 0.31764706, 0.68627451, 0.89019608) ;
#21718 = EDGE_CURVE ( 'NONE', #3266, #6431, #16009, .T. ) ;
#21719 = CARTESIAN_POINT ( 'NONE',  ( 38.58424406990786082, 159.3797705074273381, 34.21067981925357060 ) ) ;
#21720 = CYLINDRICAL_SURFACE ( 'NONE', #624, 10.00000000000000888 ) ;
#21721 = CARTESIAN_POINT ( 'NONE',  ( 11.39584491653312526, 106.7788786240791978, 8.648593811254444930 ) ) ;
#21722 = CARTESIAN_POINT ( 'NONE',  ( 41.64333658814960870, 141.7151871740940123, 38.42115945441014446 ) ) ;
#21723 = CARTESIAN_POINT ( 'NONE',  ( -143.8425227516148084, -165.6938272943107222, 55.19815736654470584 ) ) ;
#21724 = CARTESIAN_POINT ( 'NONE',  ( -151.4692556286852891, -172.4084106276440309, 59.56931450028537256 ) ) ;
#21725 = VERTEX_POINT ( 'NONE', #931 ) ;
#21726 = CARTESIAN_POINT ( 'NONE',  ( 42.21948215057684450, 78.45757658655230671, 39.21067981925355639 ) ) ;
#21727 = CARTESIAN_POINT ( 'NONE',  ( -151.4692556286852891, -158.9084106276440025, 39.74470866294723947 ) ) ;
#21728 = CARTESIAN_POINT ( 'NONE',  ( 71.19881468907274780, 122.2058620619881566, -2.419290889312981641 ) ) ;
#21729 = CARTESIAN_POINT ( 'NONE',  ( 44.55648932407425633, 112.8844580088725849, 29.45539723777780239 ) ) ;
#21730 = CARTESIAN_POINT ( 'NONE',  ( 39.42975644700377558, 122.8151871740940067, 31.60846029578754468 ) ) ;
#21731 = CARTESIAN_POINT ( 'NONE',  ( 76.67641731516037851, 114.1545672503790740, -7.227887495354823777 ) ) ;
#21732 = VERTEX_POINT ( 'NONE', #13163 ) ;
#21733 = ORIENTED_EDGE ( 'NONE', *, *, #3276, .T. ) ;
#21734 = CARTESIAN_POINT ( 'NONE',  ( 39.92123440845005433, 146.3344580088725309, 29.95742577749336988 ) ) ;
#21735 = ORIENTED_EDGE ( 'NONE', *, *, #20541, .T. ) ;
#21736 = CARTESIAN_POINT ( 'NONE',  ( 47.05648932407426344, 106.5844580088725877, 31.27175355779120025 ) ) ;
#21737 = CARTESIAN_POINT ( 'NONE',  ( 43.01140435219951286, 152.6297705074272812, 29.55568802177586107 ) ) ;
#21738 = CARTESIAN_POINT ( 'NONE',  ( 41.64333658814960870, 69.97977050742731819, 38.42115945441014446 ) ) ;
#21740 = CARTESIAN_POINT ( 'NONE',  ( 35.91077447413180579, 147.1981228300969633, 10.63281669705329691 ) ) ;
#21739 = CARTESIAN_POINT ( 'NONE',  ( 46.59305225739526435, 127.3151871740940067, 36.81289934271958941 ) ) ;
#21741 = AXIS2_PLACEMENT_3D ( 'NONE', #6763, #237, #13681 ) ;
#21742 = CARTESIAN_POINT ( 'NONE',  ( 44.55648932407425633, 77.81049967264873146, 29.45539723777780239 ) ) ;
#21743 = CARTESIAN_POINT ( 'NONE',  ( 11.08170843061617816, 132.1625483722078513, 16.49545033792581350 ) ) ;
#21744 = CARTESIAN_POINT ( 'NONE',  ( 46.10157429594899270, 97.76049967264873430, 38.46393386101375711 ) ) ;
#21745 = DIRECTION ( 'NONE',  ( -0.000000000000000000, -0.000000000000000000, -1.000000000000000000 ) ) ;
#21746 = CARTESIAN_POINT ( 'NONE',  ( 39.42975644700377558, 86.81518717409400665, 31.60846029578754468 ) ) ;
#21747 = CARTESIAN_POINT ( 'NONE',  ( 40.79384785287445681, 144.8103769814964608, 29.71740844387221259 ) ) ;
#21748 = DIRECTION ( 'NONE',  ( -0.000000000000000000, 1.000000000000000000, -0.000000000000000000 ) ) ;
#21749 = VERTEX_POINT ( 'NONE', #4447 ) ;
#21750 = CARTESIAN_POINT ( 'NONE',  ( 46.59305225739526435, 61.57977050742731251, 36.81289934271958941 ) ) ;
#21751 = CARTESIAN_POINT ( 'NONE',  ( -154.3824083646099439, -184.5584106276440650, 58.62277379824867296 ) ) ;
#21752 = CARTESIAN_POINT ( 'NONE',  ( 58.57487293839693621, 150.3975950434478648, 4.362879525569486994 ) ) ;
#21753 = CARTESIAN_POINT ( 'NONE',  ( -148.5561028927606344, -190.2584106276440536, 58.62277379824867296 ) ) ;
#21754 = ORIENTED_EDGE ( 'NONE', *, *, #18056, .T. ) ;
#21755 = CARTESIAN_POINT ( 'NONE',  ( 44.37947211624943833, 154.0151871740940237, 38.42115945441014446 ) ) ;
#21756 = EDGE_CURVE ( 'NONE', #4358, #18246, #9150, .T. ) ;
#21757 = DIRECTION ( 'NONE',  ( -0.000000000000000000, 1.000000000000000000, -0.000000000000000000 ) ) ;
#21758 = ADVANCED_FACE ( 'NONE', ( #13756 ), #17383, .T. ) ;
#21759 = CARTESIAN_POINT ( 'NONE',  ( 38.58424406990786082, 117.3797705074273097, 34.21067981925357060 ) ) ;
#21760 = CARTESIAN_POINT ( 'NONE',  ( 48.01140435219951996, 154.4344580088725820, 32.58608133808903773 ) ) ;
#21761 = AXIS2_PLACEMENT_3D ( 'NONE', #8360, #188, #6925 ) ;
#21762 = ORIENTED_EDGE ( 'NONE', *, *, #19804, .F. ) ;
#21763 = CARTESIAN_POINT ( 'NONE',  ( 14.94677925004173957, 122.6663546818147381, -4.724578312614759135 ) ) ;
#21764 = ORIENTED_EDGE ( 'NONE', *, *, #11064, .F. ) ;
#21765 = AXIS2_PLACEMENT_3D ( 'NONE', #670, #455, #12242 ) ;
#21766 = VECTOR ( 'NONE', #5014, 1000.000000000000000 ) ;
#21767 = DIRECTION ( 'NONE',  ( -0.3450121214752276400, 0.9385982292947087080, 0.000000000000000000 ) ) ;
#21768 = CARTESIAN_POINT ( 'NONE',  ( 43.01140435219951286, 155.3651871740939896, 29.55568802177586463 ) ) ;
#21769 =( BOUNDED_CURVE ( )  B_SPLINE_CURVE ( 2, ( #21364, #16607, #18384, #17928, #21698, #9579, #13199, #1189, #6598, #16386, #1521, #9473, #14741 ),
 .UNSPECIFIED., .F., .F. ) 
 B_SPLINE_CURVE_WITH_KNOTS ( ( 3, 2, 2, 2, 2, 2, 3 ),
 ( 0.9191176470588234837, 0.9205882352941175961, 0.9235294117647059320, 0.9264705882352941568, 0.9294117647058823817, 0.9323529411764706065, 0.9338235294117647189 ),
 .UNSPECIFIED. ) 
 CURVE ( )  GEOMETRIC_REPRESENTATION_ITEM ( )  RATIONAL_B_SPLINE_CURVE ( ( 0.9755282581475768211, 0.9755282581475768211, 1.000000000000000000, 0.9510565162951535312, 1.000000000000000000, 0.9510565162951535312, 1.000000000000000000, 0.9510565162951535312, 1.000000000000000000, 0.9510565162951535312, 1.000000000000000000, 0.9755282581475768211, 0.9755282581475768211 ) ) 
 REPRESENTATION_ITEM ( '' )  );
#21770 = CARTESIAN_POINT ( 'NONE',  ( 21.78317867943344766, 93.15162560046918827, 9.081842247139665147 ) ) ;
#21771 = CARTESIAN_POINT ( 'NONE',  ( 53.01140435219953417, 119.9070776186055838, 8.284271247461942878 ) ) ;
#21772 = LINE ( 'NONE', #6677, #21766 ) ;
#21773 = CARTESIAN_POINT ( 'NONE',  ( -154.5594255724347761, -180.0891397928654669, 40.14644641866476604 ) ) ;
#21774 = CARTESIAN_POINT ( 'NONE',  ( 39.92123440845005433, 90.23445800887257917, 38.46393386101375711 ) ) ;
#21775 = FACE_OUTER_BOUND ( 'NONE', #11435, .T. ) ;
#21776 = CARTESIAN_POINT ( 'NONE',  ( 46.10157429594899270, 91.76049967264873430, 38.46393386101375711 ) ) ;
#21777 = CONTEXT_DEPENDENT_SHAPE_REPRESENTATION ( #10560, #19425 ) ;
#21778 = EDGE_CURVE ( 'NONE', #18986, #19332, #18277, .T. ) ;
#21779 = CARTESIAN_POINT ( 'NONE',  ( 39.42975644700377558, 93.67977050742732104, 36.81289934271958941 ) ) ;
#21780 = CARTESIAN_POINT ( 'NONE',  ( 15.11992972970532279, 115.2318815533876375, 21.98540506394948224 ) ) ;
#21781 = CARTESIAN_POINT ( 'NONE',  ( -142.0420953463935803, -183.5438272943107449, 52.72008163687743831 ) ) ;
#21782 = CARTESIAN_POINT ( 'NONE',  ( 45.74753988029934249, 89.06518717409399244, 30.44471234641812174 ) ) ;
#21783 = DIRECTION ( 'NONE',  ( 0.000000000000000000, 0.000000000000000000, 1.000000000000000000 ) ) ;
#21784 = EDGE_LOOP ( 'NONE', ( #12802, #6016 ) ) ;
#21785 = CARTESIAN_POINT ( 'NONE',  ( -151.4692556286852891, -190.7391397928654726, 59.65701158161632378 ) ) ;
#21786 = CARTESIAN_POINT ( 'NONE',  ( 21.43032318156618388, 146.4805633285969861, 10.07716523980869816 ) ) ;
#21787 = CARTESIAN_POINT ( 'NONE',  ( 46.59305225739526435, 139.5797705074273267, 36.81289934271958941 ) ) ;
#21788 = CARTESIAN_POINT ( 'NONE',  ( 70.89290225163276205, 123.5572941793614206, -0.4820434552990647825 ) ) ;
#21789 = CARTESIAN_POINT ( 'NONE',  ( 43.01140435219951996, 10.71049967264875491, 39.21067981925356349 ) ) ;
#21790 = ORIENTED_EDGE ( 'NONE', *, *, #10936, .F. ) ;
#21791 = CARTESIAN_POINT ( 'NONE',  ( 43.01140435219951286, 149.6297705074273097, 29.55568802177586463 ) ) ;
#21792 = CARTESIAN_POINT ( 'NONE',  ( 44.37947211624943833, 95.47977050742731819, 30.00020018409699318 ) ) ;
#21793 = DIRECTION ( 'NONE',  ( 0.000000000000000000, 1.000000000000000000, -0.000000000000000000 ) ) ;
#21794 = CARTESIAN_POINT ( 'NONE',  ( 44.55648932407425633, 115.6104996726487428, 38.96596240072933170 ) ) ;
#21795 = LINE ( 'NONE', #291, #583 ) ;
#21796 = DIRECTION ( 'NONE',  ( 0.000000000000000000, 0.000000000000000000, 1.000000000000000000 ) ) ;
#21797 = CARTESIAN_POINT ( 'NONE',  ( -145.6429501568359797, -165.8438272943107279, 57.67623309621197336 ) ) ;
#21798 = CARTESIAN_POINT ( 'NONE',  ( -104.7439762501682736, 39.86119447055682485, 4.000000000000021316 ) ) ;
#21799 = CARTESIAN_POINT ( 'NONE',  ( -148.3790856849358306, -167.4630981290893033, 40.14644641866477315 ) ) ;
#21800 = CARTESIAN_POINT ( 'NONE',  ( 42.21948215057684450, 111.0373810949689926, 29.21067981925355994 ) ) ;
#21801 = CARTESIAN_POINT ( 'NONE',  ( 44.55648932407425633, 154.8844580088725991, 29.45539723777780239 ) ) ;
#21802 = CARTESIAN_POINT ( 'NONE',  ( 46.59305225739526435, 119.1797705074273068, 31.60846029578754468 ) ) ;
#21803 = CARTESIAN_POINT ( 'NONE',  ( 46.82521527361338087, 85.80558333884177102, 13.21562623509259282 ) ) ;
#21804 = CARTESIAN_POINT ( 'NONE',  ( 41.46631938032478359, 114.1104996726487428, 29.45539723777780239 ) ) ;
#21805 = CARTESIAN_POINT ( 'NONE',  ( 43.01140435219951286, 116.3651871740940038, 29.55568802177586107 ) ) ;
#21806 = DIRECTION ( 'NONE',  ( 1.000000000000000000, 0.000000000000000000, 0.000000000000000000 ) ) ;
#21807 = CARTESIAN_POINT ( 'NONE',  ( 43.01140435219951286, 125.0344580088725905, 29.21067981925356705 ) ) ;
#21808 = CARTESIAN_POINT ( 'NONE',  ( 35.49642027120339094, 86.59030162945495590, 1.581590266896775843 ) ) ;
#21809 = CARTESIAN_POINT ( 'NONE',  ( 46.66836841558743032, 147.8683539324387368, -2.938892455568735240 ) ) ;
#21810 = DIRECTION ( 'NONE',  ( -0.000000000000000000, -0.000000000000000000, -1.000000000000000000 ) ) ;
#21811 = VECTOR ( 'NONE', #16618, 1000.000000000000000 ) ;
#21812 = CARTESIAN_POINT ( 'NONE',  ( 43.01140435219951286, 86.62977050742730967, 29.55568802177586107 ) ) ;
#21813 = VERTEX_POINT ( 'NONE', #5385 ) ;
#21814 = DIRECTION ( 'NONE',  ( 1.000000000000000000, 0.000000000000000000, 0.000000000000000000 ) ) ;
#21815 = VERTEX_POINT ( 'NONE', #18833 ) ;
#21816 = CARTESIAN_POINT ( 'NONE',  ( 47.05648932407426344, 69.98445800887257917, 37.14960608071593384 ) ) ;
#21817 = DIRECTION ( 'NONE',  ( 1.000000000000000000, 0.000000000000000000, -1.734723475976805615E-16 ) ) ;
#21818 = CARTESIAN_POINT ( 'NONE',  ( -148.5561028927606344, -165.9938272943107336, 58.62277379824867296 ) ) ;
#21819 = NEXT_ASSEMBLY_USAGE_OCCURRENCE ( 'NAUO1', ' ', ' ', #16589, #17263, $ ) ;
#21820 = NEXT_ASSEMBLY_USAGE_OCCURRENCE ( 'NAUO2', ' ', ' ', #16589, #20915, $ ) ;
#21821 = NEXT_ASSEMBLY_USAGE_OCCURRENCE ( 'NAUO3', ' ', ' ', #16589, #21187, $ ) ;
#21822 = NEXT_ASSEMBLY_USAGE_OCCURRENCE ( 'NAUO4', ' ', ' ', #16589, #15648, $ ) ;
#21823 = NEXT_ASSEMBLY_USAGE_OCCURRENCE ( 'NAUO5', ' ', ' ', #16589, #11071, $ ) ;
#21824 = NEXT_ASSEMBLY_USAGE_OCCURRENCE ( 'NAUO6', ' ', ' ', #16589, #18895, $ ) ;
#21825 = NEXT_ASSEMBLY_USAGE_OCCURRENCE ( 'NAUO7', ' ', ' ', #16589, #14706, $ ) ;
#21826 = NEXT_ASSEMBLY_USAGE_OCCURRENCE ( 'NAUO8', ' ', ' ', #16589, #8803, $ ) ;
#21827 = NEXT_ASSEMBLY_USAGE_OCCURRENCE ( 'NAUO9', ' ', ' ', #16589, #8538, $ ) ;
#21828 = NEXT_ASSEMBLY_USAGE_OCCURRENCE ( 'NAUO10', ' ', ' ', #16589, #12422, $ ) ;
#21829 = NEXT_ASSEMBLY_USAGE_OCCURRENCE ( 'NAUO11', ' ', ' ', #16589, #12422, $ ) ;
#21830 = NEXT_ASSEMBLY_USAGE_OCCURRENCE ( 'NAUO12', ' ', ' ', #16589, #12422, $ ) ;
#21831 = NEXT_ASSEMBLY_USAGE_OCCURRENCE ( 'NAUO13', ' ', ' ', #16589, #12422, $ ) ;
#21832 = NEXT_ASSEMBLY_USAGE_OCCURRENCE ( 'NAUO14', ' ', ' ', #16589, #14706, $ ) ;
ENDSEC;
END-ISO-10303-21;
